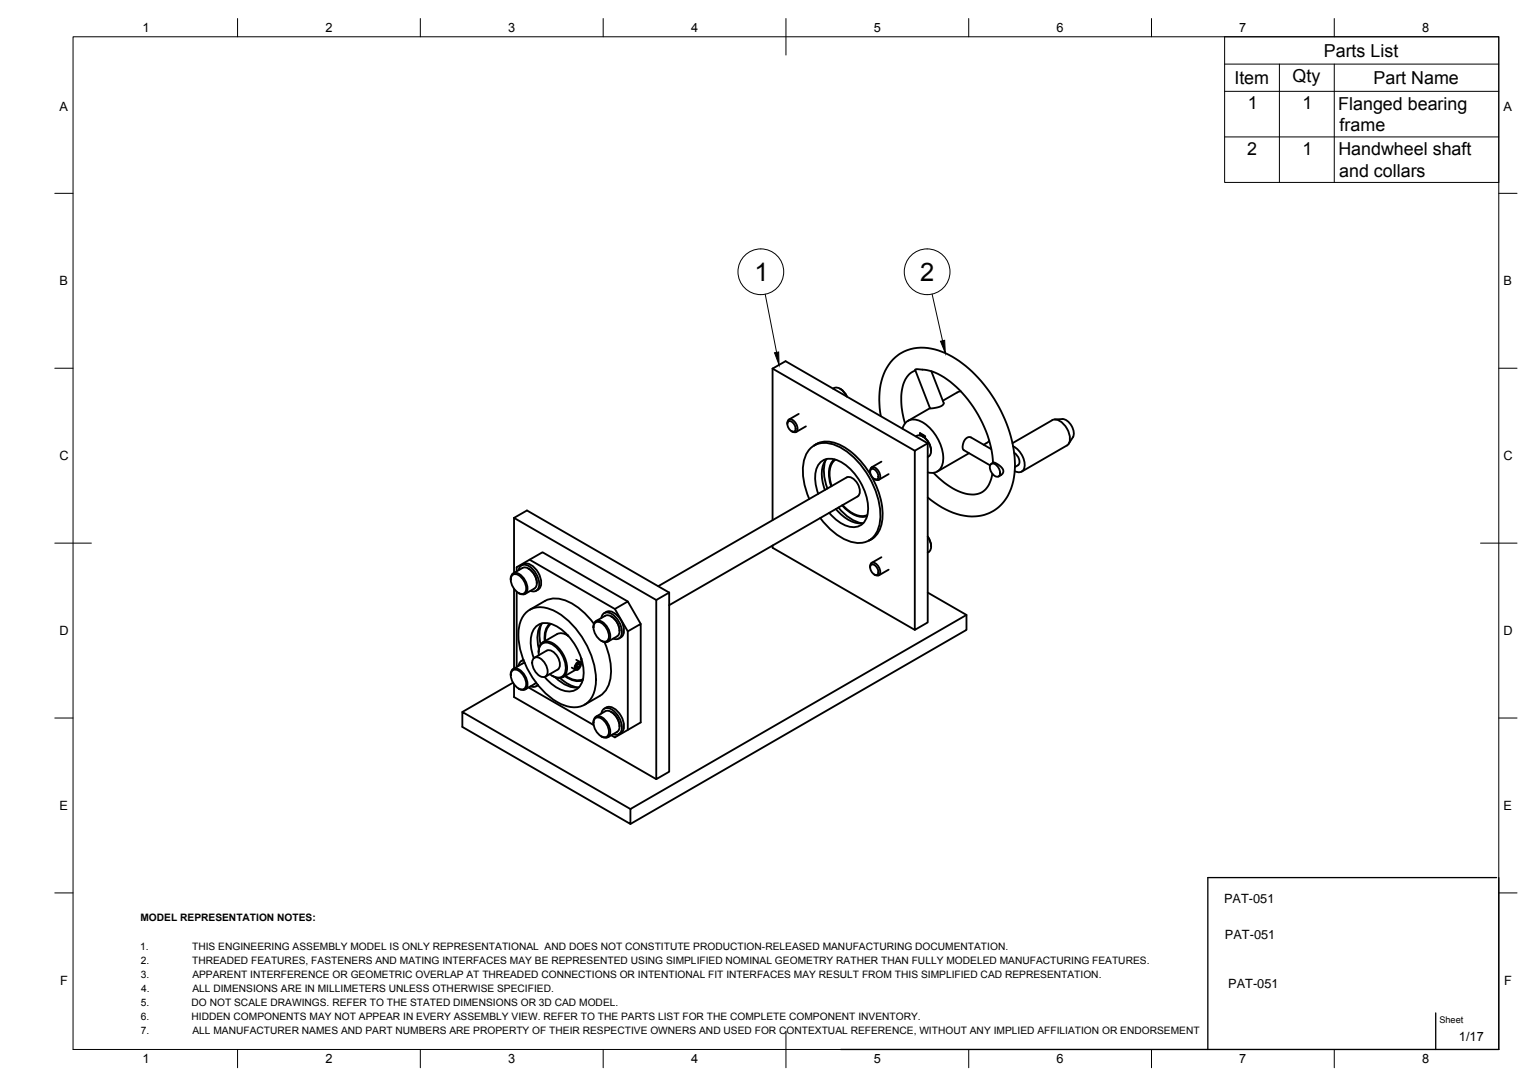
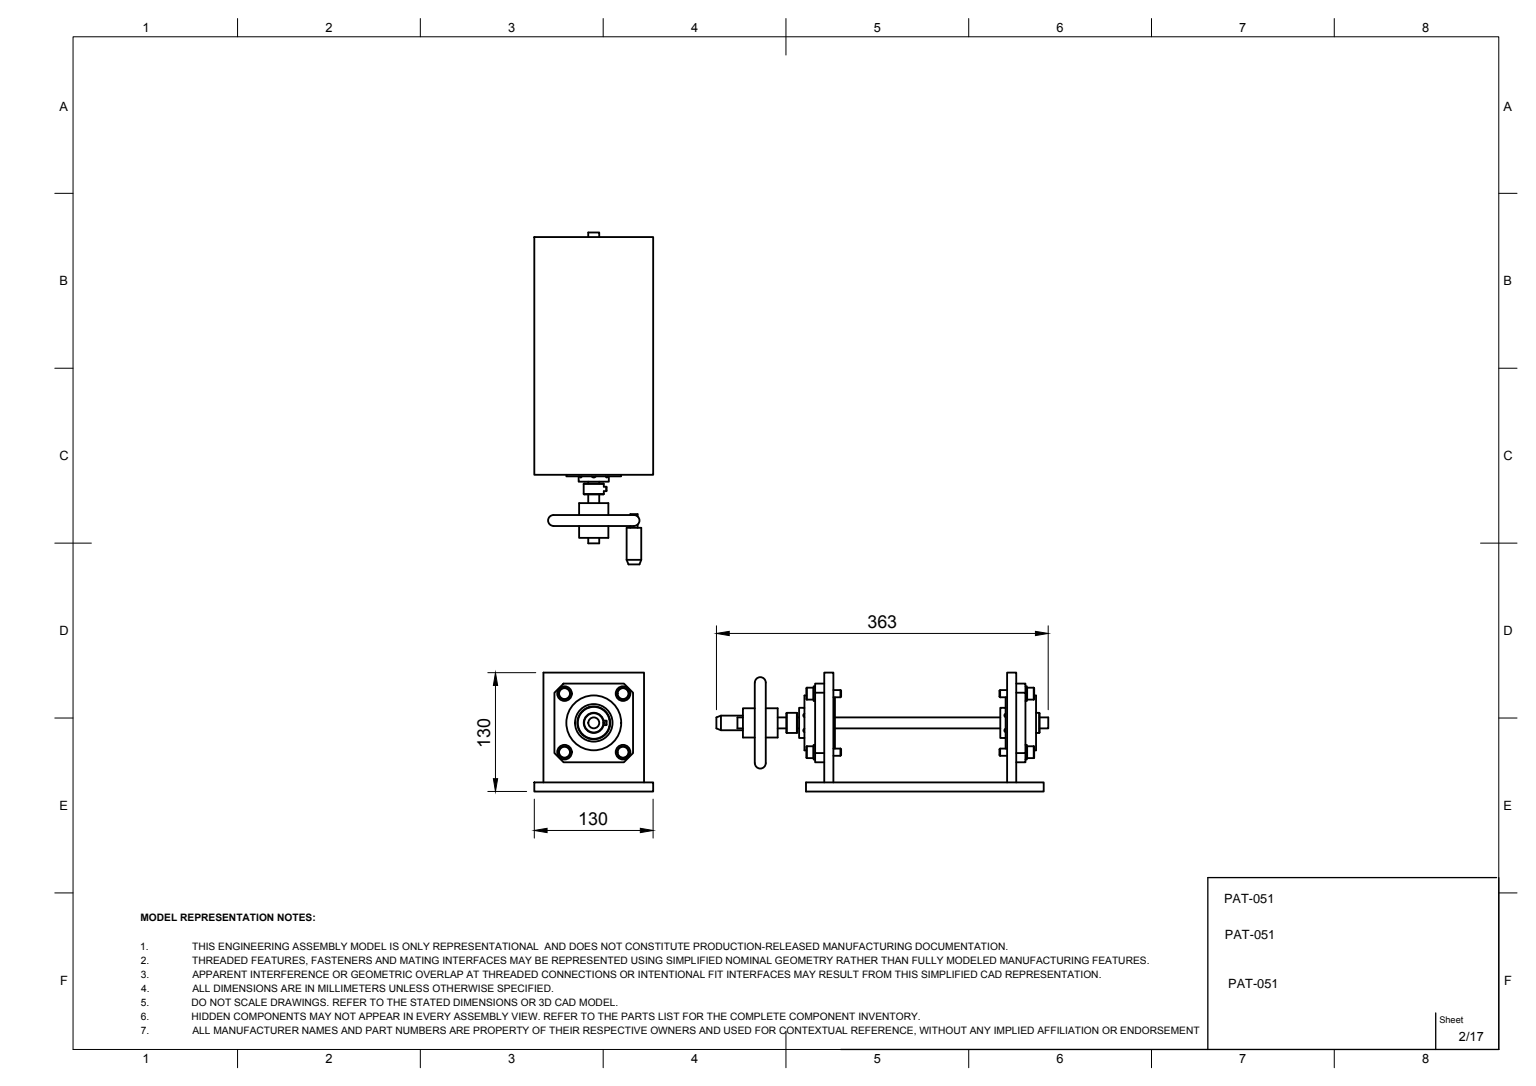
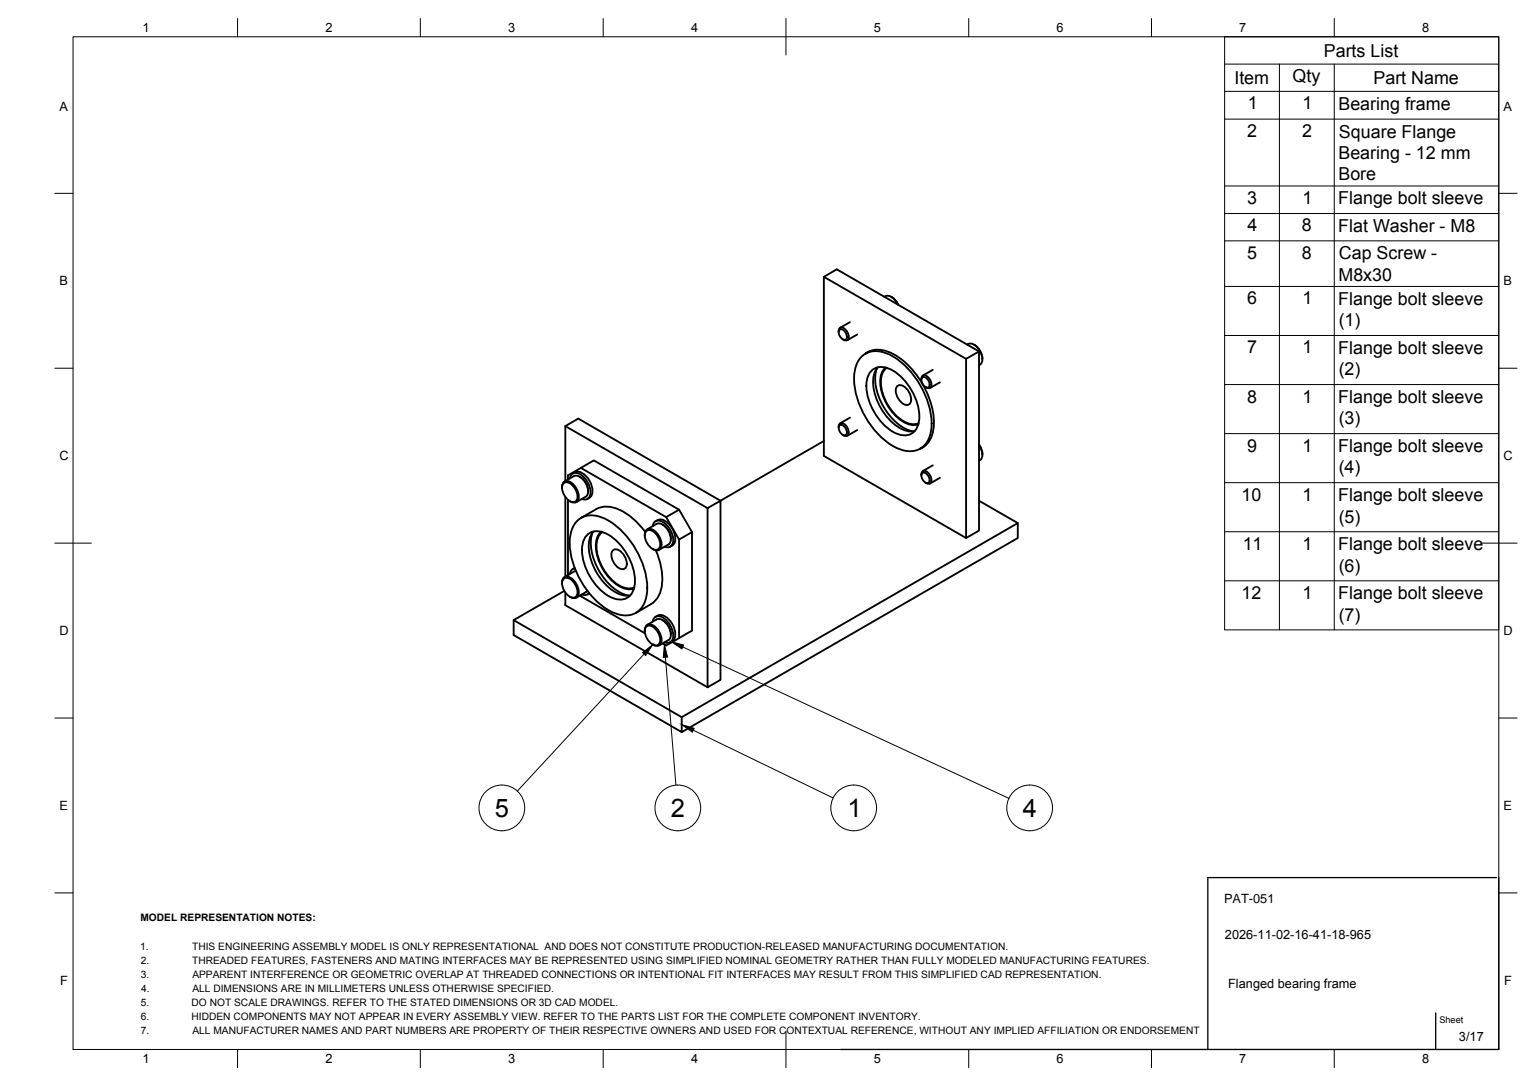
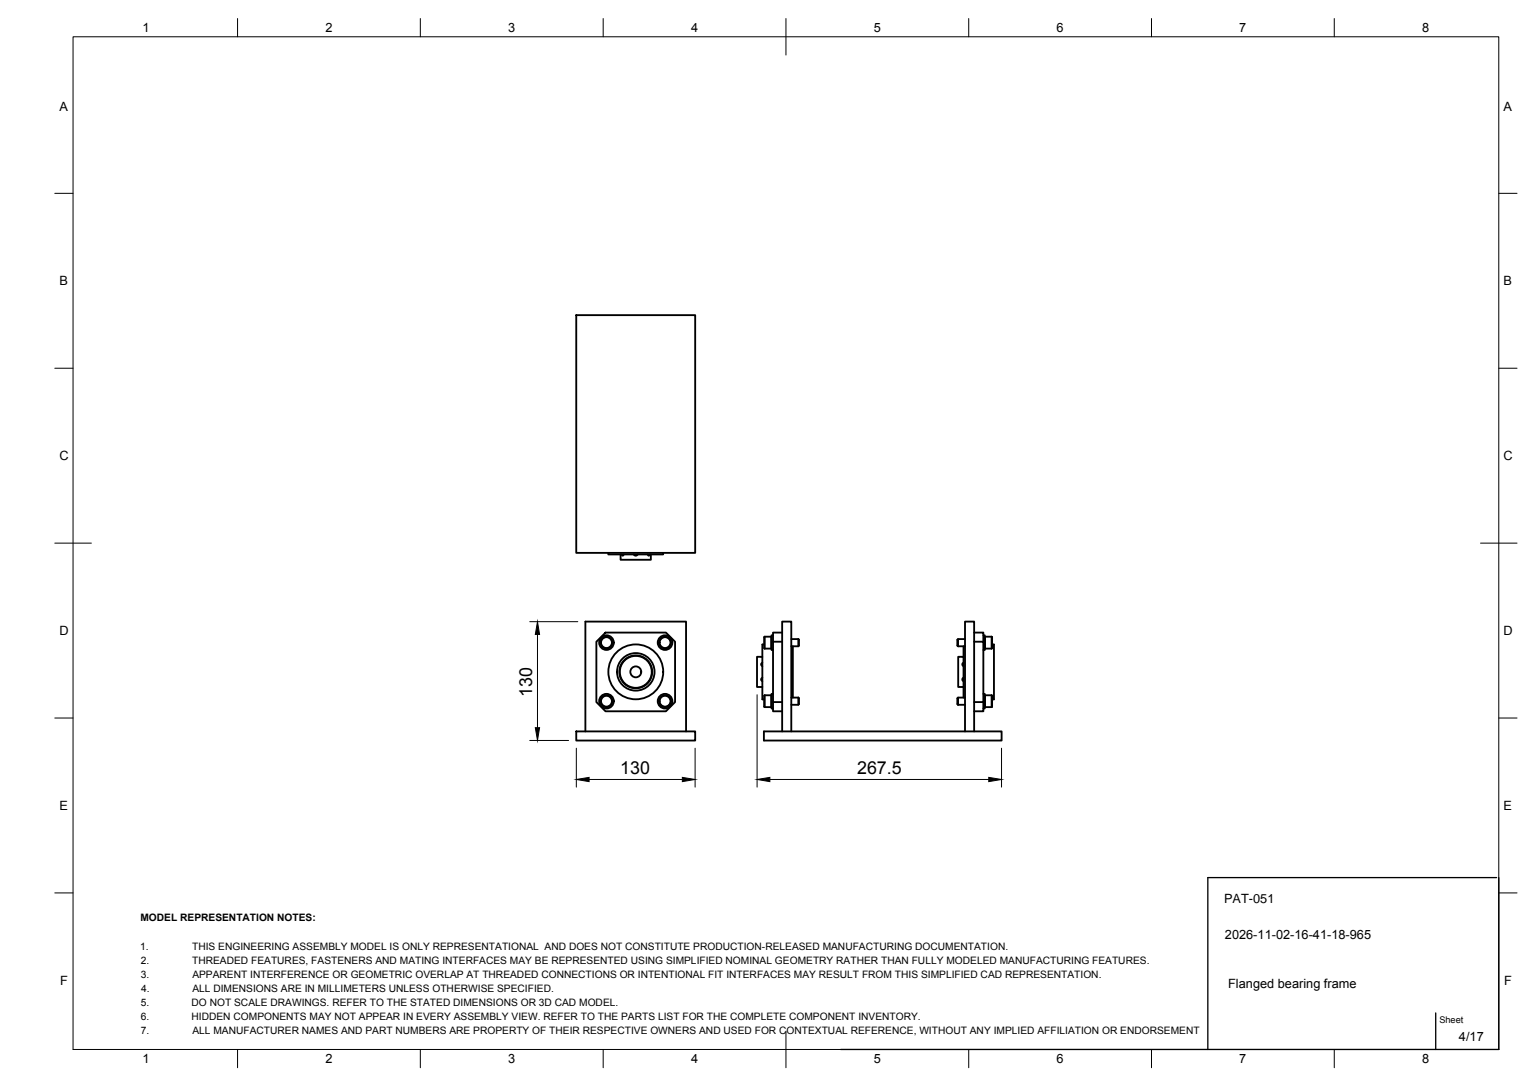
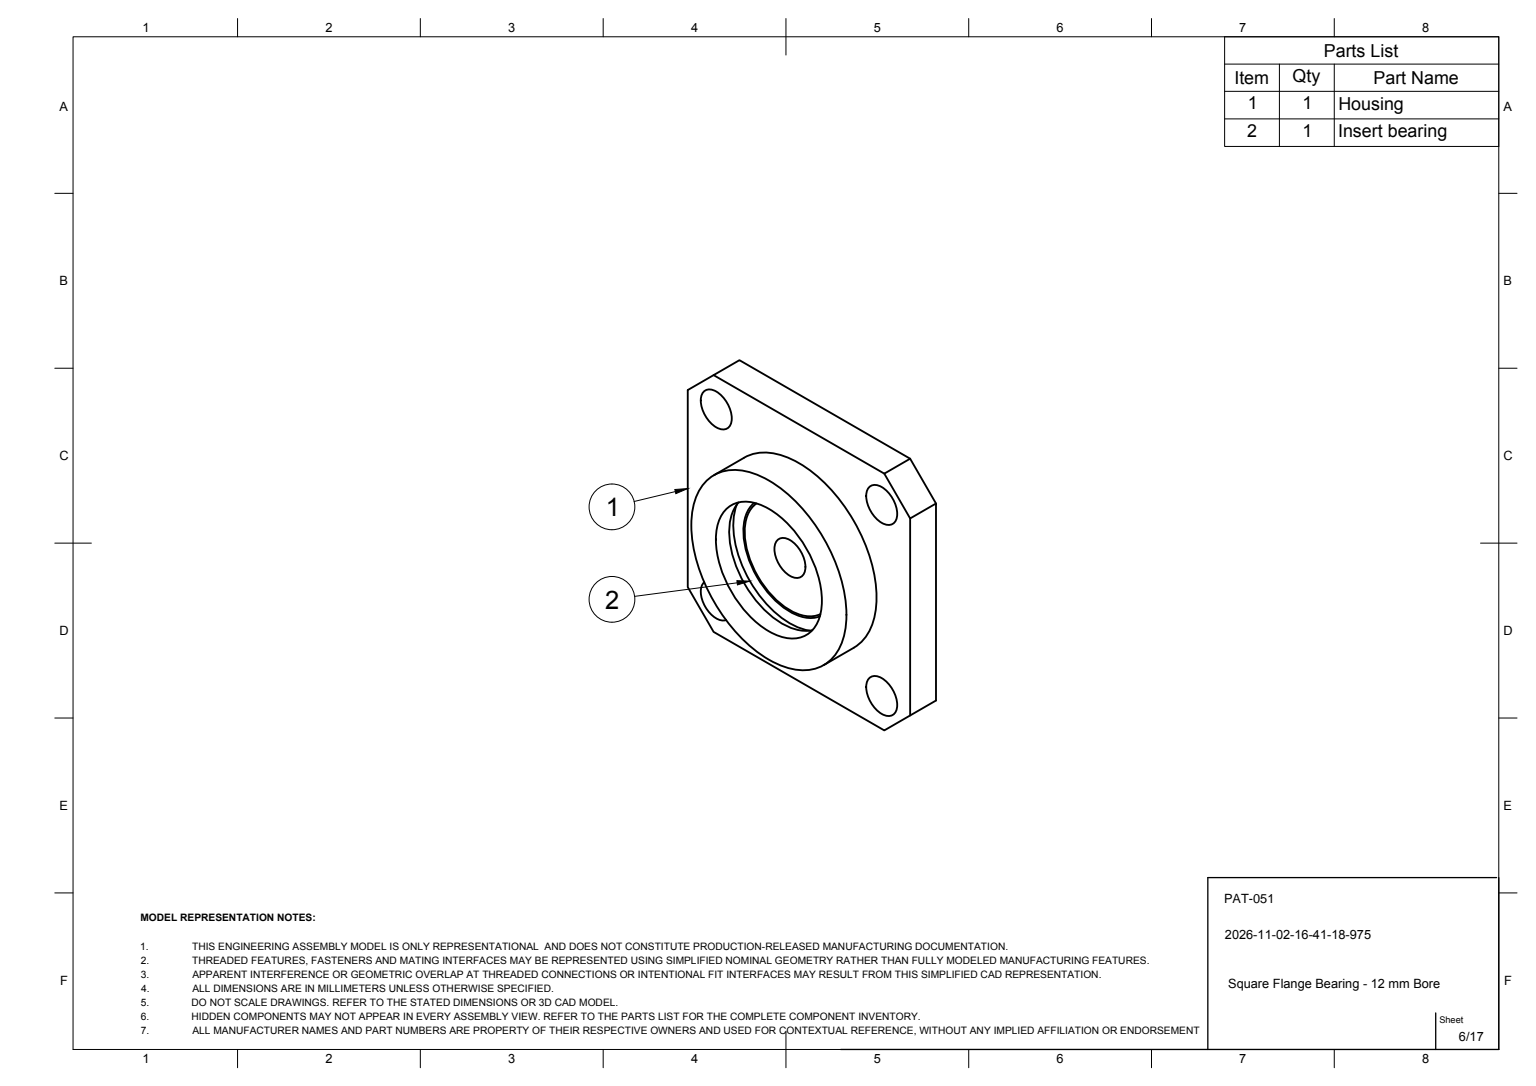
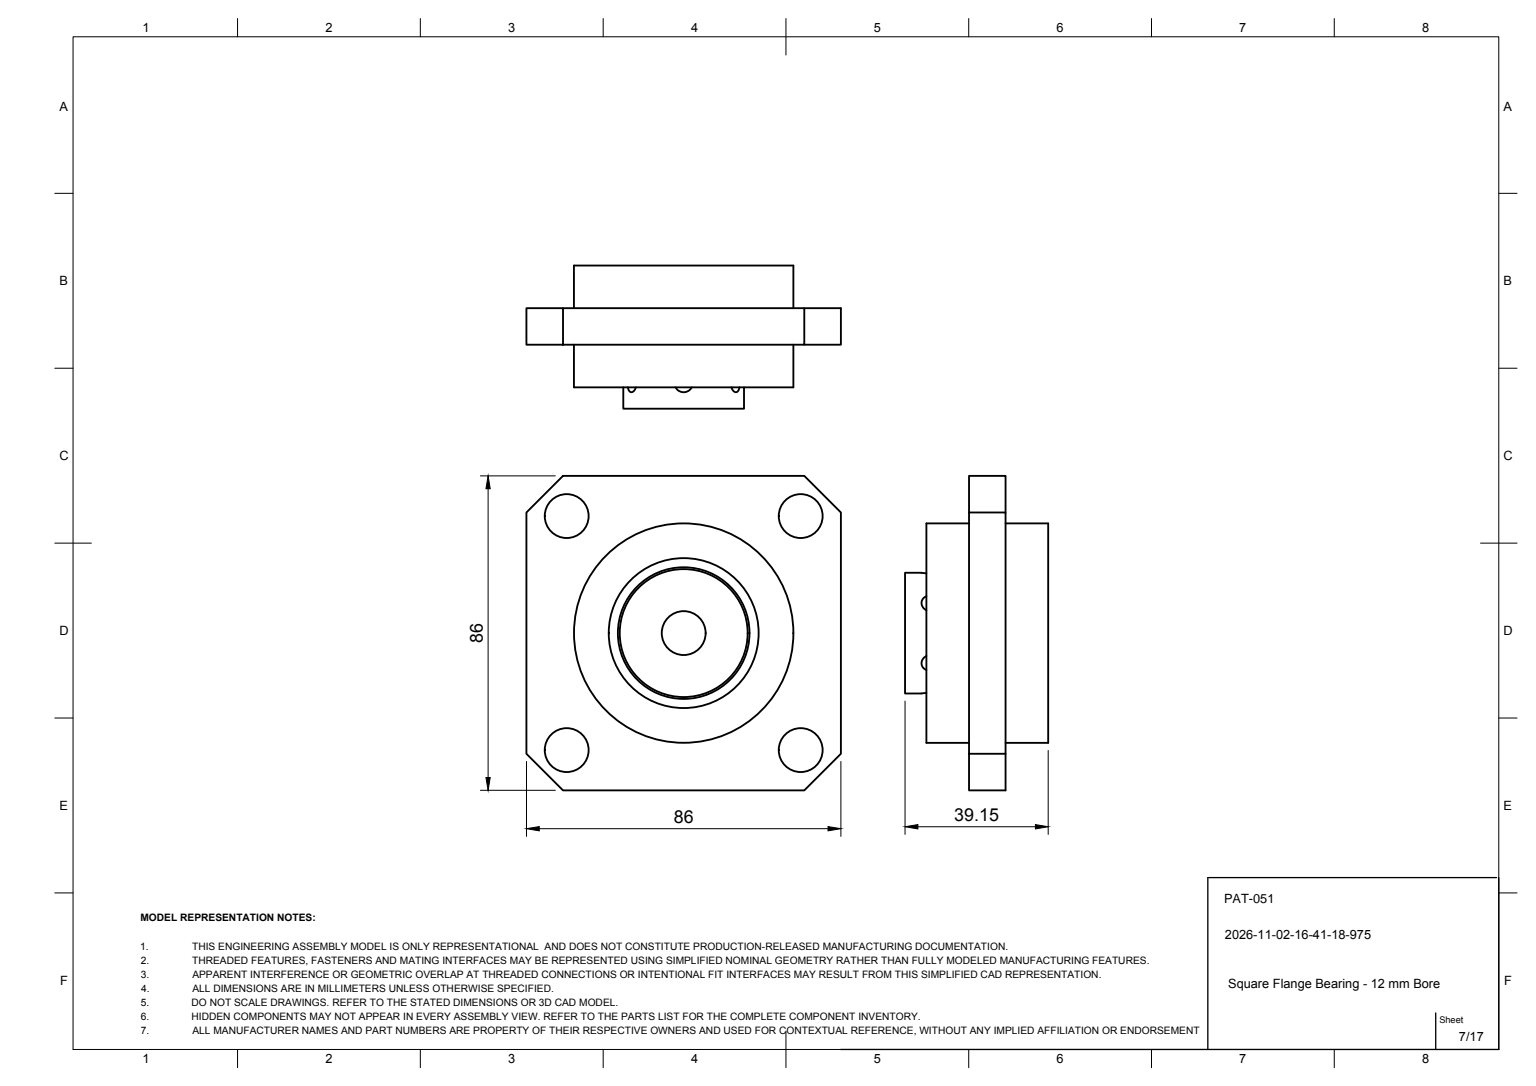
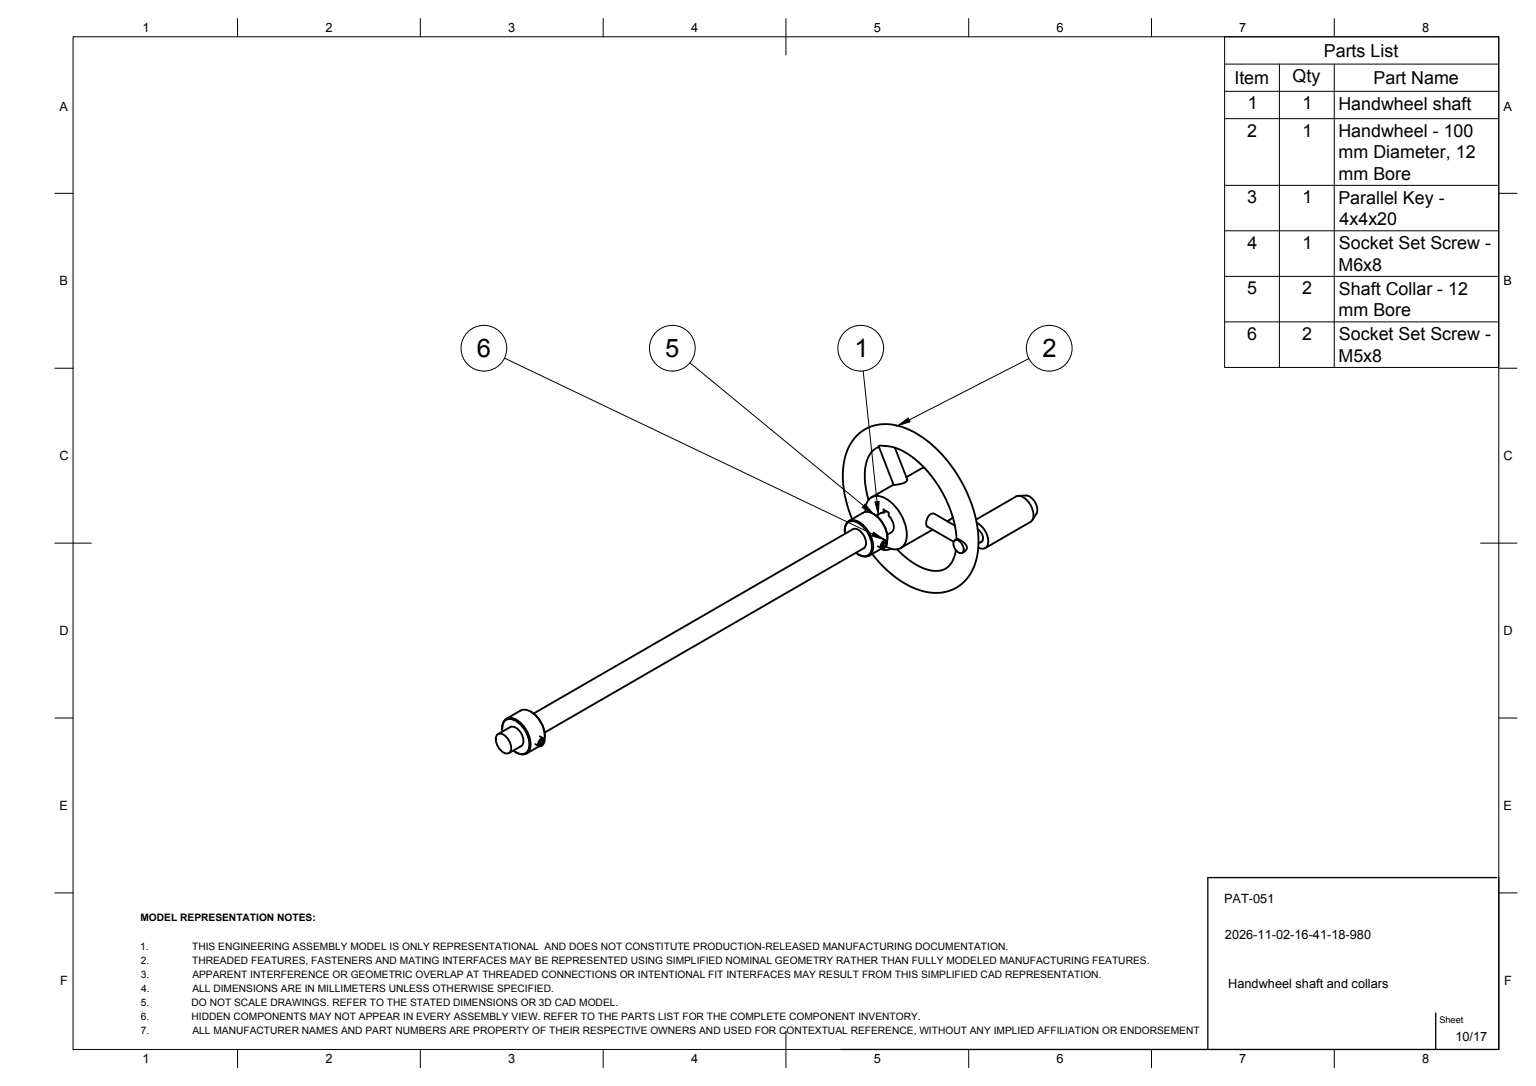
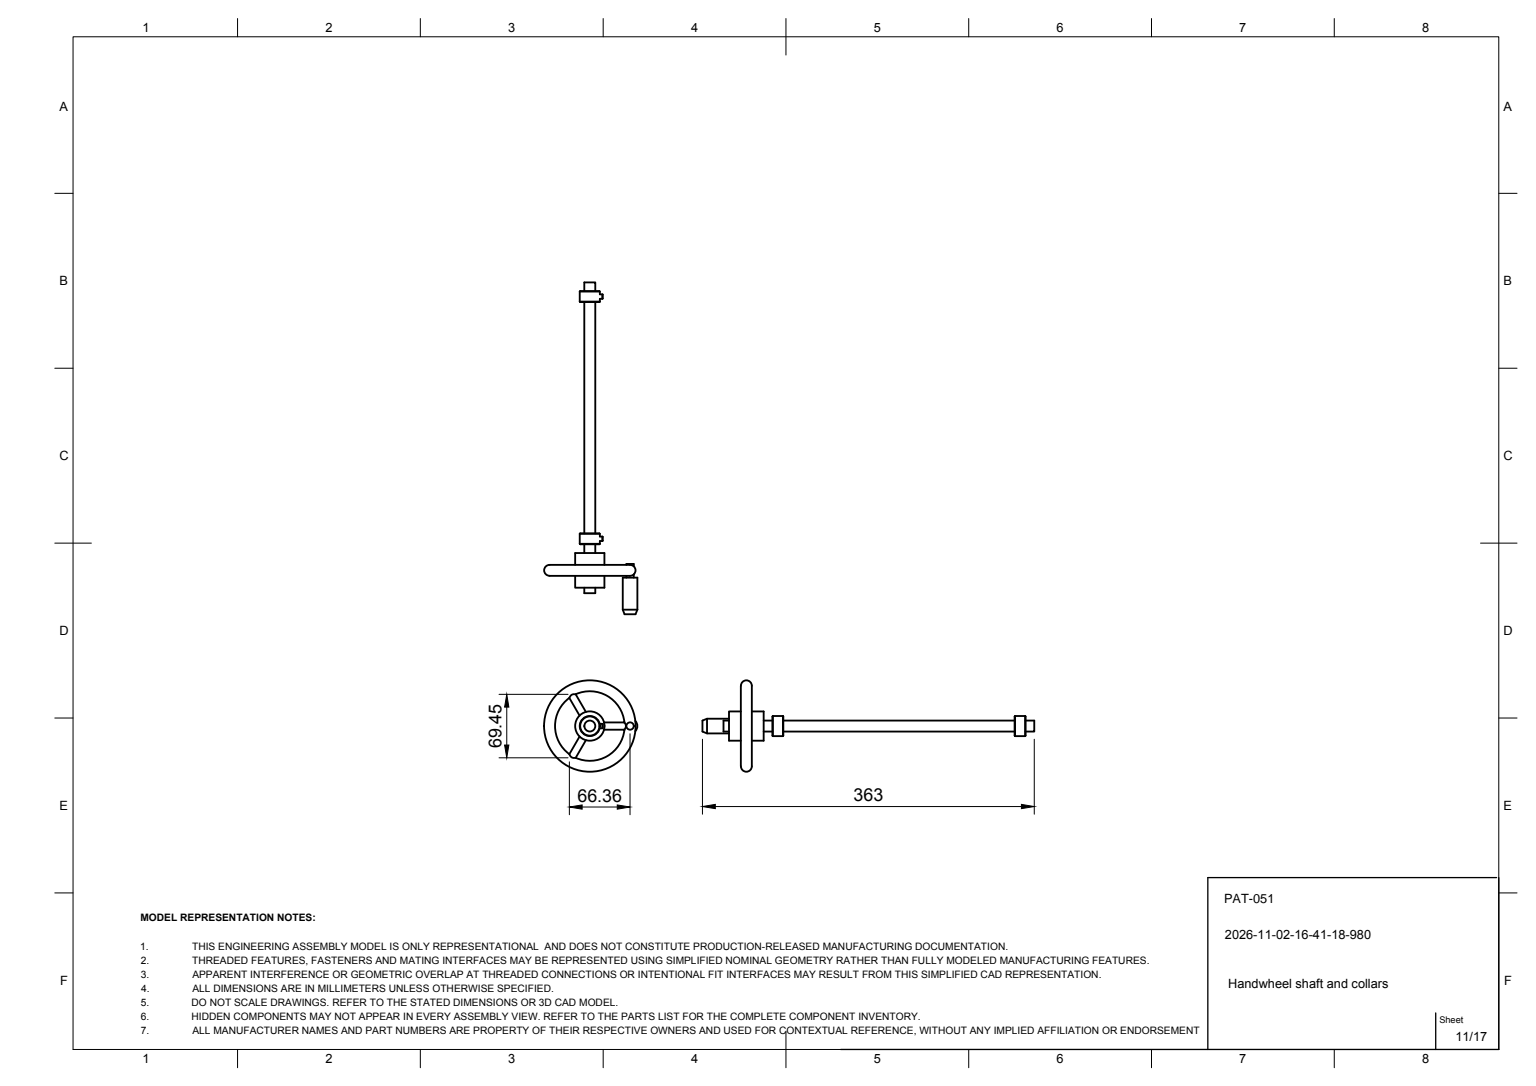
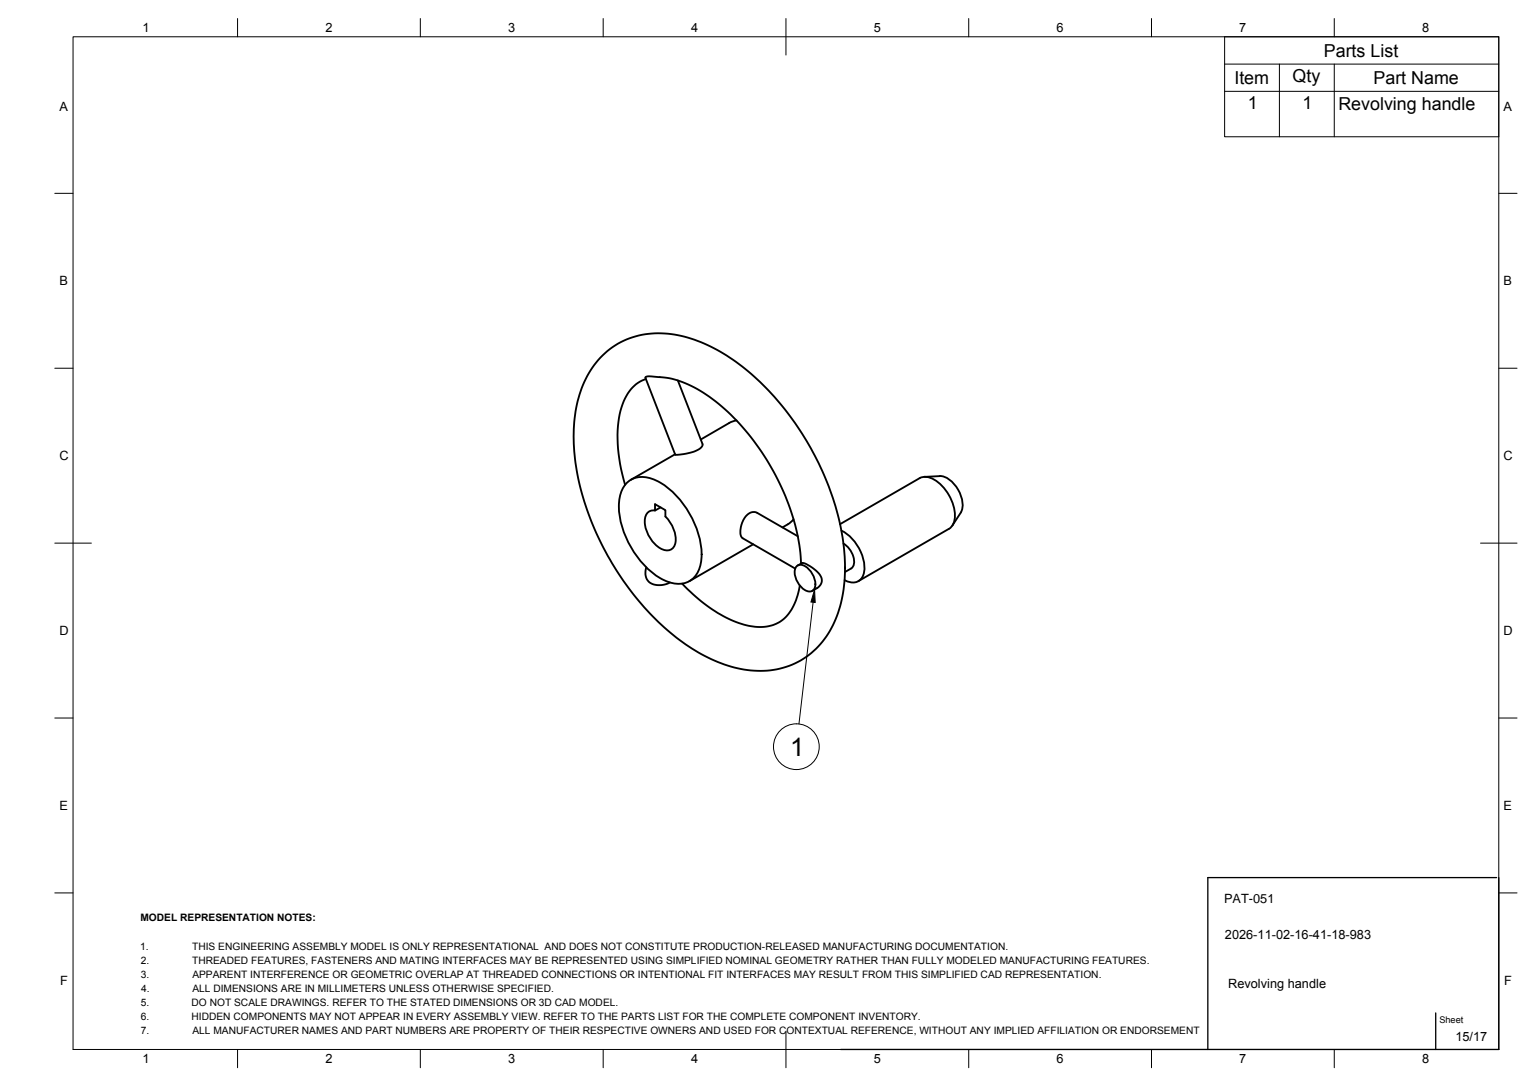
ISO-10303-21;
HEADER;
/* Generated by software containing ST-Developer
 * from STEP Tools, Inc. (www.steptools.com) 
 */

FILE_DESCRIPTION(
/* description */ ('Hand-crank flanged shaft unit'),
/* implementation_level */ '2;1');

FILE_NAME(
/* name */ 'PAT-051',
/* time_stamp */ '2026-10-27T18:35:45-07:00',
/* author */ (''),
/* organization */ (''),
/* preprocessor_version */ 'ST-DEVELOPER v20.2',
/* originating_system */ 'Autodesk Translation Framework v15.17.0.0',
/* authorisation */ '');

FILE_SCHEMA (('AUTOMOTIVE_DESIGN { 1 0 10303 214 3 1 1 }'));
ENDSEC;

DATA;
#10=MECHANICAL_DESIGN_GEOMETRIC_PRESENTATION_REPRESENTATION('',(#279,#280,
#281,#282,#283,#284,#285,#286,#287,#288,#289,#290,#291,#292,#293,#294,#295,
#296,#297,#298,#299),#6805);
#11=TOROIDAL_SURFACE('',#3848,4.4,0.6);
#12=ORIENTED_CLOSED_SHELL('',*,#3334,.F.);
#13=CONICAL_SURFACE('',#3755,0.625,0.785398163397448);
#14=CONICAL_SURFACE('',#3759,0.635,0.785398163397449);
#15=CONICAL_SURFACE('',#3763,0.41,0.463647609000806);
#16=CONICAL_SURFACE('',#3767,0.36,0.785398163397448);
#17=CONICAL_SURFACE('',#3823,0.699999999999999,0.380506377112365);
#18=CONICAL_SURFACE('',#3857,0.18,0.785398163397448);
#19=CONICAL_SURFACE('',#3861,0.18,0.785398163397448);
#20=CONICAL_SURFACE('',#3869,0.18,0.785398163397449);
#21=CONICAL_SURFACE('',#3872,0.18,0.785398163397449);
#22=CONICAL_SURFACE('',#3888,0.285,0.785398163397448);
#23=CONICAL_SURFACE('',#3892,0.25,0.785398163397448);
#24=CONICAL_SURFACE('',#3900,1.075,0.785398163397448);
#25=CONICAL_SURFACE('',#3904,1.075,0.785398163397449);
#26=CONICAL_SURFACE('',#3919,0.235,0.785398163397448);
#27=CONICAL_SURFACE('',#3923,0.2125,0.785398163397448);
#28=BREP_WITH_VOIDS('Body1',#3333,(#12));
#29=ITEM_DEFINED_TRANSFORMATION($,$,#3674,#3741);
#30=ITEM_DEFINED_TRANSFORMATION($,$,#3713,#3742);
#31=ITEM_DEFINED_TRANSFORMATION($,$,#3554,#3778);
#32=ITEM_DEFINED_TRANSFORMATION($,$,#3601,#3779);
#33=ITEM_DEFINED_TRANSFORMATION($,$,#3610,#3780);
#34=ITEM_DEFINED_TRANSFORMATION($,$,#3619,#3781);
#35=ITEM_DEFINED_TRANSFORMATION($,$,#3628,#3782);
#36=ITEM_DEFINED_TRANSFORMATION($,$,#3637,#3783);
#37=ITEM_DEFINED_TRANSFORMATION($,$,#3646,#3784);
#38=ITEM_DEFINED_TRANSFORMATION($,$,#3655,#3785);
#39=ITEM_DEFINED_TRANSFORMATION($,$,#3664,#3786);
#40=ITEM_DEFINED_TRANSFORMATION($,$,#3673,#3787);
#41=ITEM_DEFINED_TRANSFORMATION($,$,#3743,#3788);
#42=ITEM_DEFINED_TRANSFORMATION($,$,#3752,#3789);
#43=ITEM_DEFINED_TRANSFORMATION($,$,#3743,#3790);
#44=ITEM_DEFINED_TRANSFORMATION($,$,#3752,#3791);
#45=ITEM_DEFINED_TRANSFORMATION($,$,#3743,#3792);
#46=ITEM_DEFINED_TRANSFORMATION($,$,#3752,#3793);
#47=ITEM_DEFINED_TRANSFORMATION($,$,#3743,#3794);
#48=ITEM_DEFINED_TRANSFORMATION($,$,#3752,#3795);
#49=ITEM_DEFINED_TRANSFORMATION($,$,#3673,#3796);
#50=ITEM_DEFINED_TRANSFORMATION($,$,#3743,#3797);
#51=ITEM_DEFINED_TRANSFORMATION($,$,#3752,#3798);
#52=ITEM_DEFINED_TRANSFORMATION($,$,#3743,#3799);
#53=ITEM_DEFINED_TRANSFORMATION($,$,#3752,#3800);
#54=ITEM_DEFINED_TRANSFORMATION($,$,#3743,#3801);
#55=ITEM_DEFINED_TRANSFORMATION($,$,#3752,#3802);
#56=ITEM_DEFINED_TRANSFORMATION($,$,#3743,#3803);
#57=ITEM_DEFINED_TRANSFORMATION($,$,#3752,#3804);
#58=ITEM_DEFINED_TRANSFORMATION($,$,#3820,#3854);
#59=ITEM_DEFINED_TRANSFORMATION($,$,#3806,#3926);
#60=ITEM_DEFINED_TRANSFORMATION($,$,#3819,#3927);
#61=ITEM_DEFINED_TRANSFORMATION($,$,#3855,#3928);
#62=ITEM_DEFINED_TRANSFORMATION($,$,#3878,#3929);
#63=ITEM_DEFINED_TRANSFORMATION($,$,#3895,#3930);
#64=ITEM_DEFINED_TRANSFORMATION($,$,#3909,#3931);
#65=ITEM_DEFINED_TRANSFORMATION($,$,#3895,#3932);
#66=ITEM_DEFINED_TRANSFORMATION($,$,#3909,#3933);
#67=ITEM_DEFINED_TRANSFORMATION($,$,#3553,#3934);
#68=ITEM_DEFINED_TRANSFORMATION($,$,#3805,#3935);
#69=(
REPRESENTATION_RELATIONSHIP($,$,#6910,#6909)
REPRESENTATION_RELATIONSHIP_WITH_TRANSFORMATION(#29)
SHAPE_REPRESENTATION_RELATIONSHIP()
);
#70=(
REPRESENTATION_RELATIONSHIP($,$,#6911,#6909)
REPRESENTATION_RELATIONSHIP_WITH_TRANSFORMATION(#30)
SHAPE_REPRESENTATION_RELATIONSHIP()
);
#71=(
REPRESENTATION_RELATIONSHIP($,$,#6900,#6899)
REPRESENTATION_RELATIONSHIP_WITH_TRANSFORMATION(#31)
SHAPE_REPRESENTATION_RELATIONSHIP()
);
#72=(
REPRESENTATION_RELATIONSHIP($,$,#6901,#6899)
REPRESENTATION_RELATIONSHIP_WITH_TRANSFORMATION(#32)
SHAPE_REPRESENTATION_RELATIONSHIP()
);
#73=(
REPRESENTATION_RELATIONSHIP($,$,#6902,#6899)
REPRESENTATION_RELATIONSHIP_WITH_TRANSFORMATION(#33)
SHAPE_REPRESENTATION_RELATIONSHIP()
);
#74=(
REPRESENTATION_RELATIONSHIP($,$,#6903,#6899)
REPRESENTATION_RELATIONSHIP_WITH_TRANSFORMATION(#34)
SHAPE_REPRESENTATION_RELATIONSHIP()
);
#75=(
REPRESENTATION_RELATIONSHIP($,$,#6904,#6899)
REPRESENTATION_RELATIONSHIP_WITH_TRANSFORMATION(#35)
SHAPE_REPRESENTATION_RELATIONSHIP()
);
#76=(
REPRESENTATION_RELATIONSHIP($,$,#6905,#6899)
REPRESENTATION_RELATIONSHIP_WITH_TRANSFORMATION(#36)
SHAPE_REPRESENTATION_RELATIONSHIP()
);
#77=(
REPRESENTATION_RELATIONSHIP($,$,#6906,#6899)
REPRESENTATION_RELATIONSHIP_WITH_TRANSFORMATION(#37)
SHAPE_REPRESENTATION_RELATIONSHIP()
);
#78=(
REPRESENTATION_RELATIONSHIP($,$,#6907,#6899)
REPRESENTATION_RELATIONSHIP_WITH_TRANSFORMATION(#38)
SHAPE_REPRESENTATION_RELATIONSHIP()
);
#79=(
REPRESENTATION_RELATIONSHIP($,$,#6908,#6899)
REPRESENTATION_RELATIONSHIP_WITH_TRANSFORMATION(#39)
SHAPE_REPRESENTATION_RELATIONSHIP()
);
#80=(
REPRESENTATION_RELATIONSHIP($,$,#6909,#6899)
REPRESENTATION_RELATIONSHIP_WITH_TRANSFORMATION(#40)
SHAPE_REPRESENTATION_RELATIONSHIP()
);
#81=(
REPRESENTATION_RELATIONSHIP($,$,#6912,#6899)
REPRESENTATION_RELATIONSHIP_WITH_TRANSFORMATION(#41)
SHAPE_REPRESENTATION_RELATIONSHIP()
);
#82=(
REPRESENTATION_RELATIONSHIP($,$,#6913,#6899)
REPRESENTATION_RELATIONSHIP_WITH_TRANSFORMATION(#42)
SHAPE_REPRESENTATION_RELATIONSHIP()
);
#83=(
REPRESENTATION_RELATIONSHIP($,$,#6912,#6899)
REPRESENTATION_RELATIONSHIP_WITH_TRANSFORMATION(#43)
SHAPE_REPRESENTATION_RELATIONSHIP()
);
#84=(
REPRESENTATION_RELATIONSHIP($,$,#6913,#6899)
REPRESENTATION_RELATIONSHIP_WITH_TRANSFORMATION(#44)
SHAPE_REPRESENTATION_RELATIONSHIP()
);
#85=(
REPRESENTATION_RELATIONSHIP($,$,#6912,#6899)
REPRESENTATION_RELATIONSHIP_WITH_TRANSFORMATION(#45)
SHAPE_REPRESENTATION_RELATIONSHIP()
);
#86=(
REPRESENTATION_RELATIONSHIP($,$,#6913,#6899)
REPRESENTATION_RELATIONSHIP_WITH_TRANSFORMATION(#46)
SHAPE_REPRESENTATION_RELATIONSHIP()
);
#87=(
REPRESENTATION_RELATIONSHIP($,$,#6912,#6899)
REPRESENTATION_RELATIONSHIP_WITH_TRANSFORMATION(#47)
SHAPE_REPRESENTATION_RELATIONSHIP()
);
#88=(
REPRESENTATION_RELATIONSHIP($,$,#6913,#6899)
REPRESENTATION_RELATIONSHIP_WITH_TRANSFORMATION(#48)
SHAPE_REPRESENTATION_RELATIONSHIP()
);
#89=(
REPRESENTATION_RELATIONSHIP($,$,#6909,#6899)
REPRESENTATION_RELATIONSHIP_WITH_TRANSFORMATION(#49)
SHAPE_REPRESENTATION_RELATIONSHIP()
);
#90=(
REPRESENTATION_RELATIONSHIP($,$,#6912,#6899)
REPRESENTATION_RELATIONSHIP_WITH_TRANSFORMATION(#50)
SHAPE_REPRESENTATION_RELATIONSHIP()
);
#91=(
REPRESENTATION_RELATIONSHIP($,$,#6913,#6899)
REPRESENTATION_RELATIONSHIP_WITH_TRANSFORMATION(#51)
SHAPE_REPRESENTATION_RELATIONSHIP()
);
#92=(
REPRESENTATION_RELATIONSHIP($,$,#6912,#6899)
REPRESENTATION_RELATIONSHIP_WITH_TRANSFORMATION(#52)
SHAPE_REPRESENTATION_RELATIONSHIP()
);
#93=(
REPRESENTATION_RELATIONSHIP($,$,#6913,#6899)
REPRESENTATION_RELATIONSHIP_WITH_TRANSFORMATION(#53)
SHAPE_REPRESENTATION_RELATIONSHIP()
);
#94=(
REPRESENTATION_RELATIONSHIP($,$,#6912,#6899)
REPRESENTATION_RELATIONSHIP_WITH_TRANSFORMATION(#54)
SHAPE_REPRESENTATION_RELATIONSHIP()
);
#95=(
REPRESENTATION_RELATIONSHIP($,$,#6913,#6899)
REPRESENTATION_RELATIONSHIP_WITH_TRANSFORMATION(#55)
SHAPE_REPRESENTATION_RELATIONSHIP()
);
#96=(
REPRESENTATION_RELATIONSHIP($,$,#6912,#6899)
REPRESENTATION_RELATIONSHIP_WITH_TRANSFORMATION(#56)
SHAPE_REPRESENTATION_RELATIONSHIP()
);
#97=(
REPRESENTATION_RELATIONSHIP($,$,#6913,#6899)
REPRESENTATION_RELATIONSHIP_WITH_TRANSFORMATION(#57)
SHAPE_REPRESENTATION_RELATIONSHIP()
);
#98=(
REPRESENTATION_RELATIONSHIP($,$,#6917,#6916)
REPRESENTATION_RELATIONSHIP_WITH_TRANSFORMATION(#58)
SHAPE_REPRESENTATION_RELATIONSHIP()
);
#99=(
REPRESENTATION_RELATIONSHIP($,$,#6915,#6914)
REPRESENTATION_RELATIONSHIP_WITH_TRANSFORMATION(#59)
SHAPE_REPRESENTATION_RELATIONSHIP()
);
#100=(
REPRESENTATION_RELATIONSHIP($,$,#6916,#6914)
REPRESENTATION_RELATIONSHIP_WITH_TRANSFORMATION(#60)
SHAPE_REPRESENTATION_RELATIONSHIP()
);
#101=(
REPRESENTATION_RELATIONSHIP($,$,#6918,#6914)
REPRESENTATION_RELATIONSHIP_WITH_TRANSFORMATION(#61)
SHAPE_REPRESENTATION_RELATIONSHIP()
);
#102=(
REPRESENTATION_RELATIONSHIP($,$,#6919,#6914)
REPRESENTATION_RELATIONSHIP_WITH_TRANSFORMATION(#62)
SHAPE_REPRESENTATION_RELATIONSHIP()
);
#103=(
REPRESENTATION_RELATIONSHIP($,$,#6920,#6914)
REPRESENTATION_RELATIONSHIP_WITH_TRANSFORMATION(#63)
SHAPE_REPRESENTATION_RELATIONSHIP()
);
#104=(
REPRESENTATION_RELATIONSHIP($,$,#6921,#6914)
REPRESENTATION_RELATIONSHIP_WITH_TRANSFORMATION(#64)
SHAPE_REPRESENTATION_RELATIONSHIP()
);
#105=(
REPRESENTATION_RELATIONSHIP($,$,#6920,#6914)
REPRESENTATION_RELATIONSHIP_WITH_TRANSFORMATION(#65)
SHAPE_REPRESENTATION_RELATIONSHIP()
);
#106=(
REPRESENTATION_RELATIONSHIP($,$,#6921,#6914)
REPRESENTATION_RELATIONSHIP_WITH_TRANSFORMATION(#66)
SHAPE_REPRESENTATION_RELATIONSHIP()
);
#107=(
REPRESENTATION_RELATIONSHIP($,$,#6899,#6898)
REPRESENTATION_RELATIONSHIP_WITH_TRANSFORMATION(#67)
SHAPE_REPRESENTATION_RELATIONSHIP()
);
#108=(
REPRESENTATION_RELATIONSHIP($,$,#6914,#6898)
REPRESENTATION_RELATIONSHIP_WITH_TRANSFORMATION(#68)
SHAPE_REPRESENTATION_RELATIONSHIP()
);
#109=CONTEXT_DEPENDENT_SHAPE_REPRESENTATION(#69,#6848);
#110=CONTEXT_DEPENDENT_SHAPE_REPRESENTATION(#70,#6849);
#111=CONTEXT_DEPENDENT_SHAPE_REPRESENTATION(#71,#6852);
#112=CONTEXT_DEPENDENT_SHAPE_REPRESENTATION(#72,#6853);
#113=CONTEXT_DEPENDENT_SHAPE_REPRESENTATION(#73,#6854);
#114=CONTEXT_DEPENDENT_SHAPE_REPRESENTATION(#74,#6855);
#115=CONTEXT_DEPENDENT_SHAPE_REPRESENTATION(#75,#6856);
#116=CONTEXT_DEPENDENT_SHAPE_REPRESENTATION(#76,#6857);
#117=CONTEXT_DEPENDENT_SHAPE_REPRESENTATION(#77,#6858);
#118=CONTEXT_DEPENDENT_SHAPE_REPRESENTATION(#78,#6859);
#119=CONTEXT_DEPENDENT_SHAPE_REPRESENTATION(#79,#6860);
#120=CONTEXT_DEPENDENT_SHAPE_REPRESENTATION(#80,#6861);
#121=CONTEXT_DEPENDENT_SHAPE_REPRESENTATION(#81,#6862);
#122=CONTEXT_DEPENDENT_SHAPE_REPRESENTATION(#82,#6863);
#123=CONTEXT_DEPENDENT_SHAPE_REPRESENTATION(#83,#6864);
#124=CONTEXT_DEPENDENT_SHAPE_REPRESENTATION(#84,#6865);
#125=CONTEXT_DEPENDENT_SHAPE_REPRESENTATION(#85,#6866);
#126=CONTEXT_DEPENDENT_SHAPE_REPRESENTATION(#86,#6867);
#127=CONTEXT_DEPENDENT_SHAPE_REPRESENTATION(#87,#6868);
#128=CONTEXT_DEPENDENT_SHAPE_REPRESENTATION(#88,#6869);
#129=CONTEXT_DEPENDENT_SHAPE_REPRESENTATION(#89,#6870);
#130=CONTEXT_DEPENDENT_SHAPE_REPRESENTATION(#90,#6871);
#131=CONTEXT_DEPENDENT_SHAPE_REPRESENTATION(#91,#6872);
#132=CONTEXT_DEPENDENT_SHAPE_REPRESENTATION(#92,#6873);
#133=CONTEXT_DEPENDENT_SHAPE_REPRESENTATION(#93,#6874);
#134=CONTEXT_DEPENDENT_SHAPE_REPRESENTATION(#94,#6875);
#135=CONTEXT_DEPENDENT_SHAPE_REPRESENTATION(#95,#6876);
#136=CONTEXT_DEPENDENT_SHAPE_REPRESENTATION(#96,#6877);
#137=CONTEXT_DEPENDENT_SHAPE_REPRESENTATION(#97,#6878);
#138=CONTEXT_DEPENDENT_SHAPE_REPRESENTATION(#98,#6883);
#139=CONTEXT_DEPENDENT_SHAPE_REPRESENTATION(#99,#6888);
#140=CONTEXT_DEPENDENT_SHAPE_REPRESENTATION(#100,#6889);
#141=CONTEXT_DEPENDENT_SHAPE_REPRESENTATION(#101,#6890);
#142=CONTEXT_DEPENDENT_SHAPE_REPRESENTATION(#102,#6891);
#143=CONTEXT_DEPENDENT_SHAPE_REPRESENTATION(#103,#6892);
#144=CONTEXT_DEPENDENT_SHAPE_REPRESENTATION(#104,#6893);
#145=CONTEXT_DEPENDENT_SHAPE_REPRESENTATION(#105,#6894);
#146=CONTEXT_DEPENDENT_SHAPE_REPRESENTATION(#106,#6895);
#147=CONTEXT_DEPENDENT_SHAPE_REPRESENTATION(#107,#6896);
#148=CONTEXT_DEPENDENT_SHAPE_REPRESENTATION(#108,#6897);
#149=NEXT_ASSEMBLY_USAGE_OCCURRENCE('Housing:1','Housing:1','Housing:1',
#6934,#6935,'Housing:1');
#150=NEXT_ASSEMBLY_USAGE_OCCURRENCE('Insert bearing:1',
'Insert bearing:1','Insert bearing:1',#6934,#6936,'Insert bearing:1');
#151=NEXT_ASSEMBLY_USAGE_OCCURRENCE('Bearing frame:1','Bearing frame:1',
'Bearing frame:1',#6924,#6925,'Bearing frame:1');
#152=NEXT_ASSEMBLY_USAGE_OCCURRENCE('Flange bolt sleeve:1',
'Flange bolt sleeve:1','Flange bolt sleeve:1',#6924,#6926,
'Flange bolt sleeve:1');
#153=NEXT_ASSEMBLY_USAGE_OCCURRENCE('Flange bolt sleeve (1):1',
'Flange bolt sleeve (1):1','Flange bolt sleeve (1):1',#6924,#6927,
'Flange bolt sleeve (1):1');
#154=NEXT_ASSEMBLY_USAGE_OCCURRENCE('Flange bolt sleeve (2):1',
'Flange bolt sleeve (2):1','Flange bolt sleeve (2):1',#6924,#6928,
'Flange bolt sleeve (2):1');
#155=NEXT_ASSEMBLY_USAGE_OCCURRENCE('Flange bolt sleeve (3):1',
'Flange bolt sleeve (3):1','Flange bolt sleeve (3):1',#6924,#6929,
'Flange bolt sleeve (3):1');
#156=NEXT_ASSEMBLY_USAGE_OCCURRENCE('Flange bolt sleeve (4):1',
'Flange bolt sleeve (4):1','Flange bolt sleeve (4):1',#6924,#6930,
'Flange bolt sleeve (4):1');
#157=NEXT_ASSEMBLY_USAGE_OCCURRENCE('Flange bolt sleeve (5):1',
'Flange bolt sleeve (5):1','Flange bolt sleeve (5):1',#6924,#6931,
'Flange bolt sleeve (5):1');
#158=NEXT_ASSEMBLY_USAGE_OCCURRENCE('Flange bolt sleeve (6):1',
'Flange bolt sleeve (6):1','Flange bolt sleeve (6):1',#6924,#6932,
'Flange bolt sleeve (6):1');
#159=NEXT_ASSEMBLY_USAGE_OCCURRENCE('Flange bolt sleeve (7):1',
'Flange bolt sleeve (7):1','Flange bolt sleeve (7):1',#6924,#6933,
'Flange bolt sleeve (7):1');
#160=NEXT_ASSEMBLY_USAGE_OCCURRENCE(
'Square Flange Bearing - 12 mm Bore:2',
'Square Flange Bearing - 12 mm Bore:2',
'Square Flange Bearing - 12 mm Bore:2',#6924,#6934,
'Square Flange Bearing - 12 mm Bore:2');
#161=NEXT_ASSEMBLY_USAGE_OCCURRENCE('Flat Washer - M8:2',
'Flat Washer - M8:2','Flat Washer - M8:2',#6924,#6937,
'Flat Washer - M8:2');
#162=NEXT_ASSEMBLY_USAGE_OCCURRENCE('Cap Screw - M8x30:2',
'Cap Screw - M8x30:2','Cap Screw - M8x30:2',#6924,#6938,
'Cap Screw - M8x30:2');
#163=NEXT_ASSEMBLY_USAGE_OCCURRENCE('Flat Washer - M8:3',
'Flat Washer - M8:3','Flat Washer - M8:3',#6924,#6937,
'Flat Washer - M8:3');
#164=NEXT_ASSEMBLY_USAGE_OCCURRENCE('Cap Screw - M8x30:3',
'Cap Screw - M8x30:3','Cap Screw - M8x30:3',#6924,#6938,
'Cap Screw - M8x30:3');
#165=NEXT_ASSEMBLY_USAGE_OCCURRENCE('Flat Washer - M8:4',
'Flat Washer - M8:4','Flat Washer - M8:4',#6924,#6937,
'Flat Washer - M8:4');
#166=NEXT_ASSEMBLY_USAGE_OCCURRENCE('Cap Screw - M8x30:4',
'Cap Screw - M8x30:4','Cap Screw - M8x30:4',#6924,#6938,
'Cap Screw - M8x30:4');
#167=NEXT_ASSEMBLY_USAGE_OCCURRENCE('Flat Washer - M8:5',
'Flat Washer - M8:5','Flat Washer - M8:5',#6924,#6937,
'Flat Washer - M8:5');
#168=NEXT_ASSEMBLY_USAGE_OCCURRENCE('Cap Screw - M8x30:5',
'Cap Screw - M8x30:5','Cap Screw - M8x30:5',#6924,#6938,
'Cap Screw - M8x30:5');
#169=NEXT_ASSEMBLY_USAGE_OCCURRENCE(
'Square Flange Bearing - 12 mm Bore:3',
'Square Flange Bearing - 12 mm Bore:3',
'Square Flange Bearing - 12 mm Bore:3',#6924,#6934,
'Square Flange Bearing - 12 mm Bore:3');
#170=NEXT_ASSEMBLY_USAGE_OCCURRENCE('Flat Washer - M8:6',
'Flat Washer - M8:6','Flat Washer - M8:6',#6924,#6937,
'Flat Washer - M8:6');
#171=NEXT_ASSEMBLY_USAGE_OCCURRENCE('Cap Screw - M8x30:6',
'Cap Screw - M8x30:6','Cap Screw - M8x30:6',#6924,#6938,
'Cap Screw - M8x30:6');
#172=NEXT_ASSEMBLY_USAGE_OCCURRENCE('Flat Washer - M8:7',
'Flat Washer - M8:7','Flat Washer - M8:7',#6924,#6937,
'Flat Washer - M8:7');
#173=NEXT_ASSEMBLY_USAGE_OCCURRENCE('Cap Screw - M8x30:7',
'Cap Screw - M8x30:7','Cap Screw - M8x30:7',#6924,#6938,
'Cap Screw - M8x30:7');
#174=NEXT_ASSEMBLY_USAGE_OCCURRENCE('Flat Washer - M8:8',
'Flat Washer - M8:8','Flat Washer - M8:8',#6924,#6937,
'Flat Washer - M8:8');
#175=NEXT_ASSEMBLY_USAGE_OCCURRENCE('Cap Screw - M8x30:8',
'Cap Screw - M8x30:8','Cap Screw - M8x30:8',#6924,#6938,
'Cap Screw - M8x30:8');
#176=NEXT_ASSEMBLY_USAGE_OCCURRENCE('Flat Washer - M8:9',
'Flat Washer - M8:9','Flat Washer - M8:9',#6924,#6937,
'Flat Washer - M8:9');
#177=NEXT_ASSEMBLY_USAGE_OCCURRENCE('Cap Screw - M8x30:9',
'Cap Screw - M8x30:9','Cap Screw - M8x30:9',#6924,#6938,
'Cap Screw - M8x30:9');
#178=NEXT_ASSEMBLY_USAGE_OCCURRENCE('Revolving handle:1',
'Revolving handle:1','Revolving handle:1',#6941,#6942,
'Revolving handle:1');
#179=NEXT_ASSEMBLY_USAGE_OCCURRENCE('Handwheel shaft:1',
'Handwheel shaft:1','Handwheel shaft:1',#6939,#6940,'Handwheel shaft:1');
#180=NEXT_ASSEMBLY_USAGE_OCCURRENCE(
'Handwheel - 100 mm Diameter, 12 mm Bore:2',
'Handwheel - 100 mm Diameter, 12 mm Bore:2',
'Handwheel - 100 mm Diameter, 12 mm Bore:2',#6939,#6941,
'Handwheel - 100 mm Diameter, 12 mm Bore:2');
#181=NEXT_ASSEMBLY_USAGE_OCCURRENCE('Parallel Key - 4x4x20:2',
'Parallel Key - 4x4x20:2','Parallel Key - 4x4x20:2',#6939,#6943,
'Parallel Key - 4x4x20:2');
#182=NEXT_ASSEMBLY_USAGE_OCCURRENCE('Socket Set Screw - M6x8:2',
'Socket Set Screw - M6x8:2','Socket Set Screw - M6x8:2',#6939,#6944,
'Socket Set Screw - M6x8:2');
#183=NEXT_ASSEMBLY_USAGE_OCCURRENCE('Shaft Collar - 12 mm Bore:2',
'Shaft Collar - 12 mm Bore:2','Shaft Collar - 12 mm Bore:2',#6939,#6945,
'Shaft Collar - 12 mm Bore:2');
#184=NEXT_ASSEMBLY_USAGE_OCCURRENCE('Socket Set Screw - M5x8:2',
'Socket Set Screw - M5x8:2','Socket Set Screw - M5x8:2',#6939,#6946,
'Socket Set Screw - M5x8:2');
#185=NEXT_ASSEMBLY_USAGE_OCCURRENCE('Shaft Collar - 12 mm Bore:3',
'Shaft Collar - 12 mm Bore:3','Shaft Collar - 12 mm Bore:3',#6939,#6945,
'Shaft Collar - 12 mm Bore:3');
#186=NEXT_ASSEMBLY_USAGE_OCCURRENCE('Socket Set Screw - M5x8:3',
'Socket Set Screw - M5x8:3','Socket Set Screw - M5x8:3',#6939,#6946,
'Socket Set Screw - M5x8:3');
#187=NEXT_ASSEMBLY_USAGE_OCCURRENCE('Flanged bearing frame:1',
'Flanged bearing frame:1','Flanged bearing frame:1',#6923,#6924,
'Flanged bearing frame:1');
#188=NEXT_ASSEMBLY_USAGE_OCCURRENCE('Handwheel shaft and collars:1',
'Handwheel shaft and collars:1','Handwheel shaft and collars:1',#6923,#6939,
'Handwheel shaft and collars:1');
#189=B_SPLINE_CURVE_WITH_KNOTS('',3,(#5317,#5318,#5319,#5320,#5321,#5322,
#5323,#5324,#5325,#5326),.UNSPECIFIED.,.F.,.F.,(4,2,2,2,4),(1.13193471301885,
1.22626174930539,1.32058878559194,1.41491753480854,1.50924628402513),
 .UNSPECIFIED.);
#190=B_SPLINE_CURVE_WITH_KNOTS('',3,(#5328,#5329,#5330,#5331,#5332,#5333,
#5334,#5335,#5336,#5337,#5338,#5339,#5340,#5341,#5342,#5343,#5344,#5345),
 .UNSPECIFIED.,.F.,.F.,(4,2,2,2,2,2,2,2,4),(0.377311571006283,0.471638607292829,
0.565965643579376,0.66029439279597,0.754623142012565,0.84895189122916,0.943280640445754,
1.0376076767323,1.13193471301885),.UNSPECIFIED.);
#191=B_SPLINE_CURVE_WITH_KNOTS('',3,(#5346,#5347,#5348,#5349,#5350,#5351,
#5352,#5353,#5354,#5355),.UNSPECIFIED.,.F.,.F.,(4,2,2,2,4),(1.50924628402513,
1.60357503324173,1.69790378245832,1.79223081874487,1.88655785503141),
 .UNSPECIFIED.);
#192=B_SPLINE_CURVE_WITH_KNOTS('',3,(#5358,#5359,#5360,#5361,#5362,#5363,
#5364,#5365,#5366,#5367,#5368,#5369,#5370,#5371,#5372,#5373,#5374,#5375,
#5376,#5377,#5378,#5379,#5380,#5381,#5382,#5383,#5384,#5385,#5386,#5387,
#5388,#5389,#5390,#5391),.UNSPECIFIED.,.T.,.F.,(4,2,2,2,2,2,2,2,2,2,2,2,
2,2,2,2,4),(0.,0.0955080856649705,0.191016171329941,0.286408845249646,0.38180151916935,
0.477194193089055,0.572586867008759,0.66809495267373,0.763603038338701,
0.859111124003671,0.954619209668642,1.05001188358835,1.14540455750805,1.24079723142776,
1.33618990534746,1.43169799101243,1.5272060766774),.UNSPECIFIED.);
#193=B_SPLINE_CURVE_WITH_KNOTS('',3,(#5394,#5395,#5396,#5397,#5398,#5399,
#5400,#5401,#5402,#5403,#5404,#5405,#5406,#5407,#5408,#5409,#5410,#5411,
#5412,#5413,#5414,#5415,#5416,#5417,#5418,#5419,#5420,#5421,#5422,#5423,
#5424,#5425,#5426,#5427),.UNSPECIFIED.,.T.,.F.,(4,2,2,2,2,2,2,2,2,2,2,2,
2,2,2,2,4),(0.,0.0955080856649706,0.191016171329941,0.286408845249646,0.381801519169351,
0.477194193089055,0.57258686700876,0.668094952673731,0.763603038338701,
0.859111124003672,0.954619209668642,1.05001188358835,1.14540455750805,1.24079723142776,
1.33618990534746,1.43169799101243,1.5272060766774),.UNSPECIFIED.);
#194=B_SPLINE_CURVE_WITH_KNOTS('',3,(#5431,#5432,#5433,#5434,#5435,#5436,
#5437,#5438,#5439,#5440),.UNSPECIFIED.,.F.,.F.,(4,2,2,2,4),(1.13193471301885,
1.22626174930539,1.32058878559194,1.41491753480854,1.50924628402513),
 .UNSPECIFIED.);
#195=B_SPLINE_CURVE_WITH_KNOTS('',3,(#5442,#5443,#5444,#5445,#5446,#5447,
#5448,#5449,#5450,#5451,#5452,#5453,#5454,#5455,#5456,#5457,#5458,#5459),
 .UNSPECIFIED.,.F.,.F.,(4,2,2,2,2,2,2,2,4),(0.377311571006283,0.47163860729283,
0.565965643579376,0.660294392795971,0.754623142012565,0.84895189122916,
0.943280640445755,1.0376076767323,1.13193471301885),.UNSPECIFIED.);
#196=B_SPLINE_CURVE_WITH_KNOTS('',3,(#5460,#5461,#5462,#5463,#5464,#5465,
#5466,#5467,#5468,#5469),.UNSPECIFIED.,.F.,.F.,(4,2,2,2,4),(1.50924628402513,
1.60357503324173,1.69790378245832,1.79223081874487,1.88655785503141),
 .UNSPECIFIED.);
#197=B_SPLINE_CURVE_WITH_KNOTS('',3,(#5478,#5479,#5480,#5481,#5482,#5483,
#5484,#5485,#5486,#5487,#5488,#5489,#5490,#5491,#5492,#5493,#5494,#5495),
 .UNSPECIFIED.,.F.,.F.,(4,2,2,2,2,2,2,2,4),(0.377311571006282,0.471638607292829,
0.565965643579376,0.660294392795971,0.754623142012565,0.84895189122916,
0.943280640445754,1.0376076767323,1.13193471301885),.UNSPECIFIED.);
#198=B_SPLINE_CURVE_WITH_KNOTS('',3,(#5497,#5498,#5499,#5500,#5501,#5502,
#5503,#5504,#5505,#5506),.UNSPECIFIED.,.F.,.F.,(4,2,2,2,4),(1.13193471301885,
1.22626174930539,1.32058878559194,1.41491753480854,1.50924628402513),
 .UNSPECIFIED.);
#199=B_SPLINE_CURVE_WITH_KNOTS('',3,(#5507,#5508,#5509,#5510,#5511,#5512,
#5513,#5514,#5515,#5516),.UNSPECIFIED.,.F.,.F.,(4,2,2,2,4),(1.50924628402513,
1.60357503324172,1.69790378245832,1.79223081874487,1.88655785503141),
 .UNSPECIFIED.);
#200=B_SPLINE_CURVE_WITH_KNOTS('',3,(#5519,#5520,#5521,#5522,#5523,#5524,
#5525,#5526,#5527,#5528,#5529,#5530,#5531,#5532,#5533,#5534,#5535,#5536),
 .UNSPECIFIED.,.F.,.F.,(4,2,2,2,2,2,2,2,4),(0.377311571006283,0.47163860729283,
0.565965643579376,0.660294392795971,0.754623142012565,0.84895189122916,
0.943280640445754,1.0376076767323,1.13193471301885),.UNSPECIFIED.);
#201=B_SPLINE_CURVE_WITH_KNOTS('',3,(#5538,#5539,#5540,#5541,#5542,#5543,
#5544,#5545,#5546,#5547),.UNSPECIFIED.,.F.,.F.,(4,2,2,2,4),(1.13193471301885,
1.22626174930539,1.32058878559194,1.41491753480854,1.50924628402513),
 .UNSPECIFIED.);
#202=B_SPLINE_CURVE_WITH_KNOTS('',3,(#5548,#5549,#5550,#5551,#5552,#5553,
#5554,#5555,#5556,#5557),.UNSPECIFIED.,.F.,.F.,(4,2,2,2,4),(1.50924628402513,
1.60357503324173,1.69790378245832,1.79223081874487,1.88655785503141),
 .UNSPECIFIED.);
#203=B_SPLINE_CURVE_WITH_KNOTS('',3,(#5560,#5561,#5562,#5563,#5564,#5565,
#5566,#5567,#5568,#5569,#5570,#5571,#5572,#5573,#5574,#5575,#5576,#5577),
 .UNSPECIFIED.,.F.,.F.,(4,2,2,2,2,2,2,2,4),(0.377311571006282,0.471638607292829,
0.565965643579376,0.66029439279597,0.754623142012565,0.84895189122916,0.943280640445754,
1.0376076767323,1.13193471301885),.UNSPECIFIED.);
#204=B_SPLINE_CURVE_WITH_KNOTS('',3,(#5579,#5580,#5581,#5582,#5583,#5584,
#5585,#5586,#5587,#5588),.UNSPECIFIED.,.F.,.F.,(4,2,2,2,4),(1.13193471301885,
1.22626174930539,1.32058878559194,1.41491753480854,1.50924628402513),
 .UNSPECIFIED.);
#205=B_SPLINE_CURVE_WITH_KNOTS('',3,(#5589,#5590,#5591,#5592,#5593,#5594,
#5595,#5596,#5597,#5598),.UNSPECIFIED.,.F.,.F.,(4,2,2,2,4),(1.50924628402513,
1.60357503324172,1.69790378245832,1.79223081874487,1.88655785503141),
 .UNSPECIFIED.);
#206=B_SPLINE_CURVE_WITH_KNOTS('',3,(#5601,#5602,#5603,#5604,#5605,#5606,
#5607,#5608,#5609,#5610,#5611,#5612,#5613,#5614,#5615,#5616,#5617,#5618),
 .UNSPECIFIED.,.F.,.F.,(4,2,2,2,2,2,2,2,4),(0.377311571006283,0.471638607292829,
0.565965643579376,0.660294392795971,0.754623142012565,0.84895189122916,
0.943280640445755,1.0376076767323,1.13193471301885),.UNSPECIFIED.);
#207=B_SPLINE_CURVE_WITH_KNOTS('',3,(#5620,#5621,#5622,#5623,#5624,#5625,
#5626,#5627,#5628,#5629),.UNSPECIFIED.,.F.,.F.,(4,2,2,2,4),(1.13193471301885,
1.22626174930539,1.32058878559194,1.41491753480854,1.50924628402513),
 .UNSPECIFIED.);
#208=B_SPLINE_CURVE_WITH_KNOTS('',3,(#5630,#5631,#5632,#5633,#5634,#5635,
#5636,#5637,#5638,#5639),.UNSPECIFIED.,.F.,.F.,(4,2,2,2,4),(1.50924628402513,
1.60357503324172,1.69790378245832,1.79223081874487,1.88655785503141),
 .UNSPECIFIED.);
#209=B_SPLINE_CURVE_WITH_KNOTS('',3,(#5643,#5644,#5645,#5646,#5647,#5648,
#5649,#5650,#5651,#5652,#5653,#5654,#5655,#5656,#5657,#5658,#5659,#5660,
#5661,#5662,#5663,#5664,#5665,#5666,#5667,#5668,#5669,#5670,#5671,#5672,
#5673,#5674,#5675,#5676),.UNSPECIFIED.,.T.,.F.,(4,2,2,2,2,2,2,2,2,2,2,2,
2,2,2,2,4),(0.,0.0955080856649705,0.191016171329941,0.286408845249646,0.38180151916935,
0.477194193089055,0.572586867008759,0.66809495267373,0.7636030383387,0.859111124003671,
0.954619209668642,1.05001188358835,1.14540455750805,1.24079723142776,1.33618990534746,
1.43169799101243,1.5272060766774),.UNSPECIFIED.);
#210=B_SPLINE_CURVE_WITH_KNOTS('',3,(#5679,#5680,#5681,#5682,#5683,#5684,
#5685,#5686,#5687,#5688,#5689,#5690,#5691,#5692,#5693,#5694,#5695,#5696,
#5697,#5698,#5699,#5700,#5701,#5702,#5703,#5704,#5705,#5706,#5707,#5708,
#5709,#5710,#5711,#5712),.UNSPECIFIED.,.T.,.F.,(4,2,2,2,2,2,2,2,2,2,2,2,
2,2,2,2,4),(0.,0.0955080856649706,0.191016171329941,0.286408845249646,0.381801519169351,
0.477194193089055,0.57258686700876,0.668094952673731,0.763603038338701,
0.859111124003672,0.954619209668642,1.05001188358835,1.14540455750805,1.24079723142776,
1.33618990534746,1.43169799101243,1.5272060766774),.UNSPECIFIED.);
#211=B_SPLINE_CURVE_WITH_KNOTS('',3,(#5717,#5718,#5719,#5720,#5721,#5722,
#5723,#5724,#5725,#5726,#5727,#5728,#5729,#5730,#5731,#5732,#5733,#5734,
#5735,#5736,#5737,#5738,#5739,#5740,#5741,#5742,#5743,#5744,#5745,#5746,
#5747,#5748,#5749,#5750),.UNSPECIFIED.,.T.,.F.,(4,2,2,2,2,2,2,2,2,2,2,2,
2,2,2,2,4),(0.,0.0955080856649705,0.191016171329941,0.286408845249646,0.38180151916935,
0.477194193089055,0.572586867008759,0.66809495267373,0.7636030383387,0.859111124003671,
0.954619209668642,1.05001188358835,1.14540455750805,1.24079723142776,1.33618990534746,
1.43169799101243,1.5272060766774),.UNSPECIFIED.);
#212=B_SPLINE_CURVE_WITH_KNOTS('',3,(#5753,#5754,#5755,#5756,#5757,#5758,
#5759,#5760,#5761,#5762,#5763,#5764,#5765,#5766,#5767,#5768,#5769,#5770,
#5771,#5772,#5773,#5774,#5775,#5776,#5777,#5778,#5779,#5780,#5781,#5782,
#5783,#5784,#5785,#5786),.UNSPECIFIED.,.T.,.F.,(4,2,2,2,2,2,2,2,2,2,2,2,
2,2,2,2,4),(0.,0.0955080856649706,0.191016171329941,0.286408845249646,0.381801519169351,
0.477194193089055,0.57258686700876,0.668094952673731,0.763603038338701,
0.859111124003672,0.954619209668642,1.05001188358835,1.14540455750805,1.24079723142776,
1.33618990534746,1.43169799101243,1.5272060766774),.UNSPECIFIED.);
#213=B_SPLINE_CURVE_WITH_KNOTS('',3,(#5976,#5977,#5978,#5979,#5980,#5981,
#5982,#5983,#5984,#5985,#5986,#5987,#5988,#5989,#5990,#5991),
 .UNSPECIFIED.,.F.,.F.,(4,2,2,2,2,2,2,4),(-2.59552719332688,-2.57866585978924,
-2.54045071895435,-2.48749500888924,-2.3744647112323,-2.21556033801692,
-2.06580308432295,-1.95647920002804),.UNSPECIFIED.);
#214=B_SPLINE_CURVE_WITH_KNOTS('',3,(#5992,#5993,#5994,#5995,#5996,#5997,
#5998,#5999,#6000,#6001,#6002,#6003,#6004,#6005,#6006,#6007,#6008,#6009,
#6010,#6011,#6012,#6013,#6014,#6015,#6016,#6017,#6018,#6019,#6020,#6021,
#6022,#6023,#6024,#6025,#6026,#6027,#6028,#6029,#6030,#6031),
 .UNSPECIFIED.,.F.,.F.,(4,2,2,2,2,2,2,2,2,2,2,2,2,2,2,2,2,2,2,4),(-1.95647920002804,
-1.94940399731571,-1.82274564275395,-1.66864682416849,-1.54169125534598,
-1.43387376529483,-1.38209306412146,-1.34424705617005,-1.30493332486279,
-1.2460037370214,-1.10178537420969,-0.937426671253584,-0.78794048589305,
-0.665122735561945,-0.534841035694231,-0.375845726164312,-0.235011648675127,
-0.128548815843694,-0.0452999297674013,0.),.UNSPECIFIED.);
#215=B_SPLINE_CURVE_WITH_KNOTS('',3,(#6035,#6036,#6037,#6038,#6039,#6040,
#6041,#6042,#6043,#6044,#6045,#6046,#6047,#6048,#6049,#6050,#6051,#6052,
#6053,#6054,#6055,#6056,#6057,#6058,#6059,#6060,#6061,#6062,#6063,#6064,
#6065,#6066,#6067,#6068,#6069,#6070,#6071,#6072,#6073,#6074),
 .UNSPECIFIED.,.F.,.F.,(4,2,2,2,2,2,2,2,2,2,2,2,2,2,2,2,2,2,2,4),(-2.54361034519536,
-2.54253046486639,-2.4968571438888,-2.41437075183371,-2.26714492660274,
-2.09453621901679,-1.96116992397976,-1.84022994403498,-1.7037233477047,
-1.55334846612811,-1.42769894285765,-1.31373188966584,-1.26191388559973,
-1.22542262952322,-1.18873619849312,-1.1358415785305,-1.01347695720179,
-0.85748048653537,-0.726532050447263,-0.647957499864814),.UNSPECIFIED.);
#216=B_SPLINE_CURVE_WITH_KNOTS('',3,(#6075,#6076,#6077,#6078,#6079,#6080,
#6081,#6082,#6083,#6084,#6085,#6086,#6087,#6088,#6089,#6090),
 .UNSPECIFIED.,.F.,.F.,(4,2,2,2,2,2,2,4),(-0.647957499864814,-0.616035464948488,
-0.481588413072267,-0.322224684302864,-0.16030015410164,-0.0820369314872885,
-0.0377273936823807,0.),.UNSPECIFIED.);
#217=B_SPLINE_CURVE_WITH_KNOTS('',3,(#6094,#6095,#6096,#6097,#6098,#6099,
#6100,#6101,#6102,#6103,#6104,#6105,#6106,#6107,#6108,#6109,#6110,#6111),
 .UNSPECIFIED.,.F.,.F.,(4,2,2,2,2,2,2,2,4),(0.,0.0961983484640422,0.192396696928084,
0.28847519841324,0.384553699898396,0.480632201383552,0.576710702868707,
0.672909051332749,0.769107399796792),.UNSPECIFIED.);
#218=B_SPLINE_CURVE_WITH_KNOTS('',3,(#6112,#6113,#6114,#6115,#6116,#6117,
#6118,#6119,#6120,#6121,#6122,#6123,#6124,#6125,#6126,#6127,#6128,#6129),
 .UNSPECIFIED.,.F.,.F.,(4,2,2,2,2,2,2,2,4),(0.769107399796792,0.865305748260834,
0.961504096724876,1.05758259821003,1.15366109969519,1.24973960118034,1.3458181026655,
1.44201645112954,1.53821479959358),.UNSPECIFIED.);
#219=B_SPLINE_CURVE_WITH_KNOTS('',3,(#6133,#6134,#6135,#6136,#6137,#6138,
#6139,#6140,#6141,#6142),.UNSPECIFIED.,.F.,.F.,(4,2,2,2,4),(0.380002694880465,
0.475002363724097,0.570002032567729,0.66500371116433,0.760005389760931),
 .UNSPECIFIED.);
#220=B_SPLINE_CURVE_WITH_KNOTS('',3,(#6144,#6145,#6146,#6147,#6148,#6149,
#6150,#6151,#6152,#6153),.UNSPECIFIED.,.F.,.F.,(4,2,2,2,4),(0.,0.0950016785966008,
0.190003357193202,0.285003026036833,0.380002694880465),.UNSPECIFIED.);
#221=B_SPLINE_CURVE_WITH_KNOTS('',3,(#6155,#6156,#6157,#6158,#6159,#6160,
#6161,#6162,#6163,#6164),.UNSPECIFIED.,.F.,.F.,(4,2,2,2,4),(1.1400080846414,
1.23500775348503,1.33000742232866,1.42500910092526,1.52001077952186),
 .UNSPECIFIED.);
#222=B_SPLINE_CURVE_WITH_KNOTS('',3,(#6165,#6166,#6167,#6168,#6169,#6170,
#6171,#6172,#6173,#6174),.UNSPECIFIED.,.F.,.F.,(4,2,2,2,4),(0.760005389760931,
0.855007068357531,0.950008746954132,1.04500841579776,1.1400080846414),
 .UNSPECIFIED.);
#223=B_SPLINE_CURVE_WITH_KNOTS('',3,(#6205,#6206,#6207,#6208,#6209,#6210,
#6211,#6212,#6213,#6214,#6215,#6216,#6217,#6218),.UNSPECIFIED.,.F.,.F.,
(4,2,2,2,2,2,4),(-2.54850355944817,-2.47147966009112,-2.35116278368337,
-2.17207383157567,-2.03290678540533,-1.91210887606818,-1.90533893688978),
 .UNSPECIFIED.);
#224=B_SPLINE_CURVE_WITH_KNOTS('',3,(#6220,#6221,#6222,#6223,#6224,#6225,
#6226,#6227,#6228,#6229,#6230,#6231),.UNSPECIFIED.,.F.,.F.,(4,2,2,2,2,4),
(-0.637276313354589,-0.528249228810808,-0.380873908763749,-0.202177241884586,
-0.0799314225938296,0.),.UNSPECIFIED.);
#225=B_SPLINE_CURVE_WITH_KNOTS('',3,(#6234,#6235,#6236,#6237,#6238,#6239,
#6240,#6241,#6242,#6243,#6244,#6245,#6246,#6247,#6248,#6249,#6250,#6251,
#6252,#6253,#6254,#6255,#6256,#6257,#6258,#6259,#6260,#6261,#6262,#6263,
#6264,#6265,#6266,#6267),.UNSPECIFIED.,.T.,.F.,(4,2,2,2,2,2,2,2,2,2,2,2,
2,2,2,2,4),(0.,0.151379292814069,0.302758585628139,0.454116712920023,0.605474840211907,
0.756832967503791,0.908191094795676,1.05957038760974,1.21094968042381,1.36232897323788,
1.51370826605195,1.66506639334384,1.81642452063572,1.96778264792761,2.11914077521949,
2.27052006803356,2.42189936084763),.UNSPECIFIED.);
#226=B_SPLINE_CURVE_WITH_KNOTS('',3,(#6268,#6269,#6270,#6271,#6272,#6273,
#6274,#6275,#6276,#6277,#6278,#6279,#6280,#6281,#6282,#6283,#6284,#6285,
#6286,#6287,#6288,#6289,#6290,#6291),.UNSPECIFIED.,.F.,.F.,(4,2,2,2,2,2,
2,2,2,2,2,4),(-1.90533893688978,-1.78642522838365,-1.63371704918402,-1.47883830887698,
-1.3527241089287,-1.27308869766128,-1.19599240460016,-1.08166165023207,
-0.90752604130311,-0.769338857038376,-0.650696729228082,-0.637276313354589),
 .UNSPECIFIED.);
#227=B_SPLINE_CURVE_WITH_KNOTS('',3,(#6295,#6296,#6297,#6298,#6299,#6300,
#6301,#6302,#6303,#6304,#6305,#6306,#6307,#6308),.UNSPECIFIED.,.F.,.F.,
(4,2,2,2,2,2,4),(-2.5485035594474,-2.47147966009035,-2.35116278368264,-2.17207383157505,
-2.0329067854048,-1.91210887606772,-1.90533893688933),.UNSPECIFIED.);
#228=B_SPLINE_CURVE_WITH_KNOTS('',3,(#6310,#6311,#6312,#6313,#6314,#6315,
#6316,#6317,#6318,#6319,#6320,#6321),.UNSPECIFIED.,.F.,.F.,(4,2,2,2,2,4),
(-0.637276313354588,-0.528249228810783,-0.380873908763716,-0.202177241884562,
-0.0799314225938254,0.),.UNSPECIFIED.);
#229=B_SPLINE_CURVE_WITH_KNOTS('',3,(#6324,#6325,#6326,#6327,#6328,#6329,
#6330,#6331,#6332,#6333,#6334,#6335,#6336,#6337,#6338,#6339,#6340,#6341,
#6342,#6343,#6344,#6345,#6346,#6347,#6348,#6349,#6350,#6351,#6352,#6353,
#6354,#6355,#6356,#6357),.UNSPECIFIED.,.T.,.F.,(4,2,2,2,2,2,2,2,2,2,2,2,
2,2,2,2,4),(0.,0.151379292814069,0.302758585628139,0.454116712920023,0.605474840211907,
0.756832967503791,0.908191094795675,1.05957038760974,1.21094968042381,1.36232897323788,
1.51370826605195,1.66506639334384,1.81642452063572,1.9677826479276,2.11914077521949,
2.27052006803356,2.42189936084763),.UNSPECIFIED.);
#230=B_SPLINE_CURVE_WITH_KNOTS('',3,(#6358,#6359,#6360,#6361,#6362,#6363,
#6364,#6365,#6366,#6367,#6368,#6369,#6370,#6371,#6372,#6373,#6374,#6375,
#6376,#6377,#6378,#6379,#6380,#6381),.UNSPECIFIED.,.F.,.F.,(4,2,2,2,2,2,
2,2,2,2,2,4),(-1.90533893688933,-1.78642522838326,-1.63371704918372,-1.47883830887675,
-1.35272410892854,-1.27308869766117,-1.1959924046001,-1.08166165023206,
-0.907526041303146,-0.7693388570384,-0.65069672922808,-0.637276313354588),
 .UNSPECIFIED.);
#231=B_SPLINE_CURVE_WITH_KNOTS('',3,(#6385,#6386,#6387,#6388,#6389,#6390,
#6391,#6392,#6393,#6394,#6395,#6396),.UNSPECIFIED.,.F.,.F.,(4,2,2,2,2,4),
(-2.61916424636074,-2.54165598774645,-2.39715438567385,-2.22985321946239,
-2.07412217165227,-1.96431456403181),.UNSPECIFIED.);
#232=B_SPLINE_CURVE_WITH_KNOTS('',3,(#6398,#6399,#6400,#6401,#6402,#6403,
#6404,#6405,#6406,#6407,#6408,#6409),.UNSPECIFIED.,.F.,.F.,(4,2,2,2,2,4),
(-0.649106074577762,-0.568991182312238,-0.428137419269516,-0.24870582271537,
-0.112671421215055,0.),.UNSPECIFIED.);
#233=B_SPLINE_CURVE_WITH_KNOTS('',3,(#6412,#6413,#6414,#6415,#6416,#6417,
#6418,#6419,#6420,#6421,#6422,#6423,#6424,#6425,#6426,#6427,#6428,#6429,
#6430,#6431,#6432,#6433,#6434,#6435,#6436,#6437,#6438,#6439,#6440,#6441,
#6442,#6443,#6444,#6445),.UNSPECIFIED.,.T.,.F.,(4,2,2,2,2,2,2,2,2,2,2,2,
2,2,2,2,4),(0.,0.151379292814069,0.302758585628139,0.454116712920023,0.605474840211907,
0.756832967503791,0.908191094795675,1.05957038760974,1.21094968042381,1.36232897323788,
1.51370826605195,1.66506639334384,1.81642452063572,1.96778264792761,2.11914077521949,
2.27052006803356,2.42189936084763),.UNSPECIFIED.);
#234=B_SPLINE_CURVE_WITH_KNOTS('',3,(#6446,#6447,#6448,#6449,#6450,#6451,
#6452,#6453,#6454,#6455,#6456,#6457,#6458,#6459,#6460,#6461,#6462,#6463,
#6464,#6465,#6466,#6467,#6468,#6469),.UNSPECIFIED.,.F.,.F.,(4,2,2,2,2,2,
2,2,2,2,2,4),(-1.96431456403181,-1.95510446892338,-1.83271225668806,-1.67410879488211,
-1.50389075900942,-1.37768596650605,-1.25930643549399,-1.12433269575576,
-0.949014691445703,-0.810038710964932,-0.682802605332806,-0.649106074577762),
 .UNSPECIFIED.);
#235=B_SPLINE_CURVE_WITH_KNOTS('',3,(#6600,#6601,#6602,#6603,#6604,#6605,
#6606,#6607,#6608,#6609,#6610,#6611,#6612,#6613,#6614,#6615,#6616,#6617,
#6618,#6619,#6620,#6621,#6622,#6623,#6624,#6625,#6626,#6627,#6628,#6629,
#6630,#6631,#6632,#6633),.UNSPECIFIED.,.T.,.F.,(4,2,2,2,2,2,2,2,2,2,2,2,
2,2,2,2,4),(0.,0.0805240527913139,0.161048105582628,0.241524630728584,0.322001155874541,
0.402477681020498,0.482954206166455,0.563478258957768,0.644002311749082,
0.724526364540396,0.80505041733171,0.885526942477667,0.966003467623624,
1.04647999276958,1.12695651791554,1.20748057070685,1.28800462349816),
 .UNSPECIFIED.);
#236=B_SPLINE_CURVE_WITH_KNOTS('',3,(#6636,#6637,#6638,#6639,#6640,#6641,
#6642,#6643,#6644,#6645,#6646,#6647,#6648,#6649,#6650,#6651,#6652,#6653,
#6654,#6655,#6656,#6657,#6658,#6659,#6660,#6661,#6662,#6663,#6664,#6665,
#6666,#6667,#6668,#6669),.UNSPECIFIED.,.T.,.F.,(4,2,2,2,2,2,2,2,2,2,2,2,
2,2,2,2,4),(0.,0.0799614062161292,0.159922812432258,0.239880387792505,0.319837963152752,
0.399795538512999,0.479753113873245,0.559714520089374,0.639675926305503,
0.719637332521632,0.799598738737761,0.879556314098008,0.959513889458255,
1.0394714648185,1.11942904017875,1.19939044639488,1.27935185261101),
 .UNSPECIFIED.);
#237=SPHERICAL_SURFACE('',#3681,2.35);
#238=SPHERICAL_SURFACE('',#3719,2.35);
#239=SHAPE_REPRESENTATION_RELATIONSHIP('SRR','None',#6900,#259);
#240=SHAPE_REPRESENTATION_RELATIONSHIP('SRR','None',#6901,#260);
#241=SHAPE_REPRESENTATION_RELATIONSHIP('SRR','None',#6902,#261);
#242=SHAPE_REPRESENTATION_RELATIONSHIP('SRR','None',#6903,#262);
#243=SHAPE_REPRESENTATION_RELATIONSHIP('SRR','None',#6904,#263);
#244=SHAPE_REPRESENTATION_RELATIONSHIP('SRR','None',#6905,#264);
#245=SHAPE_REPRESENTATION_RELATIONSHIP('SRR','None',#6906,#265);
#246=SHAPE_REPRESENTATION_RELATIONSHIP('SRR','None',#6907,#266);
#247=SHAPE_REPRESENTATION_RELATIONSHIP('SRR','None',#6908,#267);
#248=SHAPE_REPRESENTATION_RELATIONSHIP('SRR','None',#6910,#268);
#249=SHAPE_REPRESENTATION_RELATIONSHIP('SRR','None',#6911,#269);
#250=SHAPE_REPRESENTATION_RELATIONSHIP('SRR','None',#6912,#270);
#251=SHAPE_REPRESENTATION_RELATIONSHIP('SRR','None',#6913,#271);
#252=SHAPE_REPRESENTATION_RELATIONSHIP('SRR','None',#6915,#272);
#253=SHAPE_REPRESENTATION_RELATIONSHIP('SRR','None',#6917,#273);
#254=SHAPE_REPRESENTATION_RELATIONSHIP('SRR','None',#6916,#274);
#255=SHAPE_REPRESENTATION_RELATIONSHIP('SRR','None',#6918,#275);
#256=SHAPE_REPRESENTATION_RELATIONSHIP('SRR','None',#6919,#276);
#257=SHAPE_REPRESENTATION_RELATIONSHIP('SRR','None',#6920,#277);
#258=SHAPE_REPRESENTATION_RELATIONSHIP('SRR','None',#6921,#278);
#259=ADVANCED_BREP_SHAPE_REPRESENTATION('',(#300),#6783);
#260=ADVANCED_BREP_SHAPE_REPRESENTATION('',(#301),#6784);
#261=ADVANCED_BREP_SHAPE_REPRESENTATION('',(#302),#6785);
#262=ADVANCED_BREP_SHAPE_REPRESENTATION('',(#303),#6786);
#263=ADVANCED_BREP_SHAPE_REPRESENTATION('',(#304),#6787);
#264=ADVANCED_BREP_SHAPE_REPRESENTATION('',(#305),#6788);
#265=ADVANCED_BREP_SHAPE_REPRESENTATION('',(#306),#6789);
#266=ADVANCED_BREP_SHAPE_REPRESENTATION('',(#307),#6790);
#267=ADVANCED_BREP_SHAPE_REPRESENTATION('',(#308),#6791);
#268=ADVANCED_BREP_SHAPE_REPRESENTATION('',(#309),#6793);
#269=ADVANCED_BREP_SHAPE_REPRESENTATION('',(#310,#311),#6794);
#270=ADVANCED_BREP_SHAPE_REPRESENTATION('',(#312),#6795);
#271=ADVANCED_BREP_SHAPE_REPRESENTATION('',(#28),#6796);
#272=ADVANCED_BREP_SHAPE_REPRESENTATION('',(#313),#6798);
#273=ADVANCED_BREP_SHAPE_REPRESENTATION('',(#314),#6800);
#274=ADVANCED_BREP_SHAPE_REPRESENTATION('',(#315),#6799);
#275=ADVANCED_BREP_SHAPE_REPRESENTATION('',(#316),#6801);
#276=ADVANCED_BREP_SHAPE_REPRESENTATION('',(#317),#6802);
#277=ADVANCED_BREP_SHAPE_REPRESENTATION('',(#318),#6803);
#278=ADVANCED_BREP_SHAPE_REPRESENTATION('',(#319),#6804);
#279=STYLED_ITEM('',(#7091),#300);
#280=STYLED_ITEM('',(#7098),#301);
#281=STYLED_ITEM('',(#7098),#302);
#282=STYLED_ITEM('',(#7098),#303);
#283=STYLED_ITEM('',(#7098),#304);
#284=STYLED_ITEM('',(#7098),#305);
#285=STYLED_ITEM('',(#7098),#306);
#286=STYLED_ITEM('',(#7098),#307);
#287=STYLED_ITEM('',(#7098),#308);
#288=STYLED_ITEM('',(#7070),#309);
#289=STYLED_ITEM('',(#7091),#310);
#290=STYLED_ITEM('',(#7091),#311);
#291=STYLED_ITEM('',(#7098),#312);
#292=STYLED_ITEM('',(#7098),#28);
#293=STYLED_ITEM('',(#7091),#313);
#294=STYLED_ITEM('',(#7084),#314);
#295=STYLED_ITEM('',(#7084),#315);
#296=STYLED_ITEM('',(#7091),#316);
#297=STYLED_ITEM('',(#7098),#317);
#298=STYLED_ITEM('',(#7091),#318);
#299=STYLED_ITEM('',(#7098),#319);
#300=MANIFOLD_SOLID_BREP('Body1',#3320);
#301=MANIFOLD_SOLID_BREP('Body1',#3321);
#302=MANIFOLD_SOLID_BREP('Body1',#3322);
#303=MANIFOLD_SOLID_BREP('Body1',#3323);
#304=MANIFOLD_SOLID_BREP('Body1',#3324);
#305=MANIFOLD_SOLID_BREP('Body1',#3325);
#306=MANIFOLD_SOLID_BREP('Body1',#3326);
#307=MANIFOLD_SOLID_BREP('Body1',#3327);
#308=MANIFOLD_SOLID_BREP('Body1',#3328);
#309=MANIFOLD_SOLID_BREP('Body1',#3329);
#310=MANIFOLD_SOLID_BREP('Body1',#3330);
#311=MANIFOLD_SOLID_BREP('Body2',#3331);
#312=MANIFOLD_SOLID_BREP('Body1',#3332);
#313=MANIFOLD_SOLID_BREP('Body1',#3335);
#314=MANIFOLD_SOLID_BREP('Body1',#3336);
#315=MANIFOLD_SOLID_BREP('Body1',#3337);
#316=MANIFOLD_SOLID_BREP('Body1',#3338);
#317=MANIFOLD_SOLID_BREP('Body1',#3339);
#318=MANIFOLD_SOLID_BREP('Body1',#3340);
#319=MANIFOLD_SOLID_BREP('Body1',#3341);
#320=FACE_BOUND('',#712,.T.);
#321=FACE_BOUND('',#713,.T.);
#322=FACE_BOUND('',#714,.T.);
#323=FACE_BOUND('',#715,.T.);
#324=FACE_BOUND('',#716,.T.);
#325=FACE_BOUND('',#718,.T.);
#326=FACE_BOUND('',#719,.T.);
#327=FACE_BOUND('',#720,.T.);
#328=FACE_BOUND('',#721,.T.);
#329=FACE_BOUND('',#722,.T.);
#330=FACE_BOUND('',#732,.T.);
#331=FACE_BOUND('',#733,.T.);
#332=FACE_BOUND('',#734,.T.);
#333=FACE_BOUND('',#735,.T.);
#334=FACE_BOUND('',#736,.T.);
#335=FACE_BOUND('',#738,.T.);
#336=FACE_BOUND('',#739,.T.);
#337=FACE_BOUND('',#740,.T.);
#338=FACE_BOUND('',#741,.T.);
#339=FACE_BOUND('',#742,.T.);
#340=FACE_BOUND('',#748,.T.);
#341=FACE_BOUND('',#749,.T.);
#342=FACE_BOUND('',#754,.T.);
#343=FACE_BOUND('',#756,.T.);
#344=FACE_BOUND('',#760,.T.);
#345=FACE_BOUND('',#762,.T.);
#346=FACE_BOUND('',#766,.T.);
#347=FACE_BOUND('',#768,.T.);
#348=FACE_BOUND('',#772,.T.);
#349=FACE_BOUND('',#774,.T.);
#350=FACE_BOUND('',#778,.T.);
#351=FACE_BOUND('',#780,.T.);
#352=FACE_BOUND('',#784,.T.);
#353=FACE_BOUND('',#786,.T.);
#354=FACE_BOUND('',#790,.T.);
#355=FACE_BOUND('',#792,.T.);
#356=FACE_BOUND('',#796,.T.);
#357=FACE_BOUND('',#798,.T.);
#358=FACE_BOUND('',#802,.T.);
#359=FACE_BOUND('',#803,.T.);
#360=FACE_BOUND('',#807,.T.);
#361=FACE_BOUND('',#809,.T.);
#362=FACE_BOUND('',#823,.T.);
#363=FACE_BOUND('',#824,.T.);
#364=FACE_BOUND('',#825,.T.);
#365=FACE_BOUND('',#826,.T.);
#366=FACE_BOUND('',#827,.T.);
#367=FACE_BOUND('',#829,.T.);
#368=FACE_BOUND('',#830,.T.);
#369=FACE_BOUND('',#831,.T.);
#370=FACE_BOUND('',#832,.T.);
#371=FACE_BOUND('',#833,.T.);
#372=FACE_BOUND('',#836,.T.);
#373=FACE_BOUND('',#838,.T.);
#374=FACE_BOUND('',#839,.T.);
#375=FACE_BOUND('',#841,.T.);
#376=FACE_BOUND('',#845,.T.);
#377=FACE_BOUND('',#846,.T.);
#378=FACE_BOUND('',#847,.T.);
#379=FACE_BOUND('',#848,.T.);
#380=FACE_BOUND('',#849,.T.);
#381=FACE_BOUND('',#850,.T.);
#382=FACE_BOUND('',#856,.T.);
#383=FACE_BOUND('',#858,.T.);
#384=FACE_BOUND('',#861,.T.);
#385=FACE_BOUND('',#863,.T.);
#386=FACE_BOUND('',#864,.T.);
#387=FACE_BOUND('',#865,.T.);
#388=FACE_BOUND('',#866,.T.);
#389=FACE_BOUND('',#867,.T.);
#390=FACE_BOUND('',#868,.T.);
#391=FACE_BOUND('',#872,.T.);
#392=FACE_BOUND('',#874,.T.);
#393=FACE_BOUND('',#880,.T.);
#394=FACE_BOUND('',#899,.T.);
#395=FACE_BOUND('',#906,.T.);
#396=FACE_BOUND('',#915,.T.);
#397=FACE_BOUND('',#917,.T.);
#398=FACE_BOUND('',#922,.T.);
#399=FACE_BOUND('',#924,.T.);
#400=FACE_BOUND('',#925,.T.);
#401=FACE_BOUND('',#926,.T.);
#402=FACE_BOUND('',#928,.T.);
#403=FACE_BOUND('',#929,.T.);
#404=FACE_BOUND('',#952,.T.);
#405=FACE_BOUND('',#959,.T.);
#406=FACE_BOUND('',#962,.T.);
#407=FACE_BOUND('',#965,.T.);
#408=FACE_BOUND('',#967,.T.);
#409=FACE_BOUND('',#976,.T.);
#410=PLANE('',#3570);
#411=PLANE('',#3571);
#412=PLANE('',#3572);
#413=PLANE('',#3573);
#414=PLANE('',#3574);
#415=PLANE('',#3590);
#416=PLANE('',#3591);
#417=PLANE('',#3592);
#418=PLANE('',#3593);
#419=PLANE('',#3594);
#420=PLANE('',#3595);
#421=PLANE('',#3596);
#422=PLANE('',#3597);
#423=PLANE('',#3598);
#424=PLANE('',#3599);
#425=PLANE('',#3600);
#426=PLANE('',#3608);
#427=PLANE('',#3609);
#428=PLANE('',#3617);
#429=PLANE('',#3618);
#430=PLANE('',#3626);
#431=PLANE('',#3627);
#432=PLANE('',#3635);
#433=PLANE('',#3636);
#434=PLANE('',#3644);
#435=PLANE('',#3645);
#436=PLANE('',#3653);
#437=PLANE('',#3654);
#438=PLANE('',#3662);
#439=PLANE('',#3663);
#440=PLANE('',#3671);
#441=PLANE('',#3672);
#442=PLANE('',#3689);
#443=PLANE('',#3690);
#444=PLANE('',#3703);
#445=PLANE('',#3704);
#446=PLANE('',#3705);
#447=PLANE('',#3706);
#448=PLANE('',#3707);
#449=PLANE('',#3708);
#450=PLANE('',#3709);
#451=PLANE('',#3710);
#452=PLANE('',#3711);
#453=PLANE('',#3712);
#454=PLANE('',#3717);
#455=PLANE('',#3722);
#456=PLANE('',#3732);
#457=PLANE('',#3734);
#458=PLANE('',#3738);
#459=PLANE('',#3750);
#460=PLANE('',#3751);
#461=PLANE('',#3753);
#462=PLANE('',#3761);
#463=PLANE('',#3769);
#464=PLANE('',#3770);
#465=PLANE('',#3771);
#466=PLANE('',#3772);
#467=PLANE('',#3773);
#468=PLANE('',#3774);
#469=PLANE('',#3775);
#470=PLANE('',#3776);
#471=PLANE('',#3777);
#472=PLANE('',#3807);
#473=PLANE('',#3808);
#474=PLANE('',#3810);
#475=PLANE('',#3811);
#476=PLANE('',#3812);
#477=PLANE('',#3817);
#478=PLANE('',#3818);
#479=PLANE('',#3821);
#480=PLANE('',#3827);
#481=PLANE('',#3831);
#482=PLANE('',#3834);
#483=PLANE('',#3835);
#484=PLANE('',#3836);
#485=PLANE('',#3837);
#486=PLANE('',#3845);
#487=PLANE('',#3856);
#488=PLANE('',#3860);
#489=PLANE('',#3866);
#490=PLANE('',#3867);
#491=PLANE('',#3868);
#492=PLANE('',#3871);
#493=PLANE('',#3876);
#494=PLANE('',#3877);
#495=PLANE('',#3879);
#496=PLANE('',#3880);
#497=PLANE('',#3881);
#498=PLANE('',#3882);
#499=PLANE('',#3883);
#500=PLANE('',#3884);
#501=PLANE('',#3885);
#502=PLANE('',#3886);
#503=PLANE('',#3894);
#504=PLANE('',#3897);
#505=PLANE('',#3906);
#506=PLANE('',#3910);
#507=PLANE('',#3911);
#508=PLANE('',#3912);
#509=PLANE('',#3913);
#510=PLANE('',#3914);
#511=PLANE('',#3915);
#512=PLANE('',#3916);
#513=PLANE('',#3917);
#514=PLANE('',#3925);
#515=FACE_OUTER_BOUND('',#703,.T.);
#516=FACE_OUTER_BOUND('',#704,.T.);
#517=FACE_OUTER_BOUND('',#705,.T.);
#518=FACE_OUTER_BOUND('',#706,.T.);
#519=FACE_OUTER_BOUND('',#707,.T.);
#520=FACE_OUTER_BOUND('',#708,.T.);
#521=FACE_OUTER_BOUND('',#709,.T.);
#522=FACE_OUTER_BOUND('',#710,.T.);
#523=FACE_OUTER_BOUND('',#711,.T.);
#524=FACE_OUTER_BOUND('',#717,.T.);
#525=FACE_OUTER_BOUND('',#723,.T.);
#526=FACE_OUTER_BOUND('',#724,.T.);
#527=FACE_OUTER_BOUND('',#725,.T.);
#528=FACE_OUTER_BOUND('',#726,.T.);
#529=FACE_OUTER_BOUND('',#727,.T.);
#530=FACE_OUTER_BOUND('',#728,.T.);
#531=FACE_OUTER_BOUND('',#729,.T.);
#532=FACE_OUTER_BOUND('',#730,.T.);
#533=FACE_OUTER_BOUND('',#731,.T.);
#534=FACE_OUTER_BOUND('',#737,.T.);
#535=FACE_OUTER_BOUND('',#743,.T.);
#536=FACE_OUTER_BOUND('',#744,.T.);
#537=FACE_OUTER_BOUND('',#745,.T.);
#538=FACE_OUTER_BOUND('',#746,.T.);
#539=FACE_OUTER_BOUND('',#747,.T.);
#540=FACE_OUTER_BOUND('',#750,.T.);
#541=FACE_OUTER_BOUND('',#751,.T.);
#542=FACE_OUTER_BOUND('',#752,.T.);
#543=FACE_OUTER_BOUND('',#753,.T.);
#544=FACE_OUTER_BOUND('',#755,.T.);
#545=FACE_OUTER_BOUND('',#757,.T.);
#546=FACE_OUTER_BOUND('',#758,.T.);
#547=FACE_OUTER_BOUND('',#759,.T.);
#548=FACE_OUTER_BOUND('',#761,.T.);
#549=FACE_OUTER_BOUND('',#763,.T.);
#550=FACE_OUTER_BOUND('',#764,.T.);
#551=FACE_OUTER_BOUND('',#765,.T.);
#552=FACE_OUTER_BOUND('',#767,.T.);
#553=FACE_OUTER_BOUND('',#769,.T.);
#554=FACE_OUTER_BOUND('',#770,.T.);
#555=FACE_OUTER_BOUND('',#771,.T.);
#556=FACE_OUTER_BOUND('',#773,.T.);
#557=FACE_OUTER_BOUND('',#775,.T.);
#558=FACE_OUTER_BOUND('',#776,.T.);
#559=FACE_OUTER_BOUND('',#777,.T.);
#560=FACE_OUTER_BOUND('',#779,.T.);
#561=FACE_OUTER_BOUND('',#781,.T.);
#562=FACE_OUTER_BOUND('',#782,.T.);
#563=FACE_OUTER_BOUND('',#783,.T.);
#564=FACE_OUTER_BOUND('',#785,.T.);
#565=FACE_OUTER_BOUND('',#787,.T.);
#566=FACE_OUTER_BOUND('',#788,.T.);
#567=FACE_OUTER_BOUND('',#789,.T.);
#568=FACE_OUTER_BOUND('',#791,.T.);
#569=FACE_OUTER_BOUND('',#793,.T.);
#570=FACE_OUTER_BOUND('',#794,.T.);
#571=FACE_OUTER_BOUND('',#795,.T.);
#572=FACE_OUTER_BOUND('',#797,.T.);
#573=FACE_OUTER_BOUND('',#799,.T.);
#574=FACE_OUTER_BOUND('',#800,.T.);
#575=FACE_OUTER_BOUND('',#801,.T.);
#576=FACE_OUTER_BOUND('',#804,.T.);
#577=FACE_OUTER_BOUND('',#805,.T.);
#578=FACE_OUTER_BOUND('',#806,.T.);
#579=FACE_OUTER_BOUND('',#808,.T.);
#580=FACE_OUTER_BOUND('',#810,.T.);
#581=FACE_OUTER_BOUND('',#811,.T.);
#582=FACE_OUTER_BOUND('',#812,.T.);
#583=FACE_OUTER_BOUND('',#813,.T.);
#584=FACE_OUTER_BOUND('',#814,.T.);
#585=FACE_OUTER_BOUND('',#815,.T.);
#586=FACE_OUTER_BOUND('',#816,.T.);
#587=FACE_OUTER_BOUND('',#817,.T.);
#588=FACE_OUTER_BOUND('',#818,.T.);
#589=FACE_OUTER_BOUND('',#819,.T.);
#590=FACE_OUTER_BOUND('',#820,.T.);
#591=FACE_OUTER_BOUND('',#821,.T.);
#592=FACE_OUTER_BOUND('',#822,.T.);
#593=FACE_OUTER_BOUND('',#828,.T.);
#594=FACE_OUTER_BOUND('',#834,.T.);
#595=FACE_OUTER_BOUND('',#835,.T.);
#596=FACE_OUTER_BOUND('',#837,.T.);
#597=FACE_OUTER_BOUND('',#840,.T.);
#598=FACE_OUTER_BOUND('',#842,.T.);
#599=FACE_OUTER_BOUND('',#843,.T.);
#600=FACE_OUTER_BOUND('',#844,.T.);
#601=FACE_OUTER_BOUND('',#851,.T.);
#602=FACE_OUTER_BOUND('',#852,.T.);
#603=FACE_OUTER_BOUND('',#853,.T.);
#604=FACE_OUTER_BOUND('',#854,.T.);
#605=FACE_OUTER_BOUND('',#855,.T.);
#606=FACE_OUTER_BOUND('',#857,.T.);
#607=FACE_OUTER_BOUND('',#859,.T.);
#608=FACE_OUTER_BOUND('',#860,.T.);
#609=FACE_OUTER_BOUND('',#862,.T.);
#610=FACE_OUTER_BOUND('',#869,.T.);
#611=FACE_OUTER_BOUND('',#870,.T.);
#612=FACE_OUTER_BOUND('',#871,.T.);
#613=FACE_OUTER_BOUND('',#873,.T.);
#614=FACE_OUTER_BOUND('',#875,.T.);
#615=FACE_OUTER_BOUND('',#876,.T.);
#616=FACE_OUTER_BOUND('',#877,.T.);
#617=FACE_OUTER_BOUND('',#878,.T.);
#618=FACE_OUTER_BOUND('',#879,.T.);
#619=FACE_OUTER_BOUND('',#881,.T.);
#620=FACE_OUTER_BOUND('',#882,.T.);
#621=FACE_OUTER_BOUND('',#883,.T.);
#622=FACE_OUTER_BOUND('',#884,.T.);
#623=FACE_OUTER_BOUND('',#885,.T.);
#624=FACE_OUTER_BOUND('',#886,.T.);
#625=FACE_OUTER_BOUND('',#887,.T.);
#626=FACE_OUTER_BOUND('',#888,.T.);
#627=FACE_OUTER_BOUND('',#889,.T.);
#628=FACE_OUTER_BOUND('',#890,.T.);
#629=FACE_OUTER_BOUND('',#891,.T.);
#630=FACE_OUTER_BOUND('',#892,.T.);
#631=FACE_OUTER_BOUND('',#893,.T.);
#632=FACE_OUTER_BOUND('',#894,.T.);
#633=FACE_OUTER_BOUND('',#895,.T.);
#634=FACE_OUTER_BOUND('',#896,.T.);
#635=FACE_OUTER_BOUND('',#897,.T.);
#636=FACE_OUTER_BOUND('',#898,.T.);
#637=FACE_OUTER_BOUND('',#900,.T.);
#638=FACE_OUTER_BOUND('',#901,.T.);
#639=FACE_OUTER_BOUND('',#902,.T.);
#640=FACE_OUTER_BOUND('',#903,.T.);
#641=FACE_OUTER_BOUND('',#904,.T.);
#642=FACE_OUTER_BOUND('',#905,.T.);
#643=FACE_OUTER_BOUND('',#907,.T.);
#644=FACE_OUTER_BOUND('',#908,.T.);
#645=FACE_OUTER_BOUND('',#909,.T.);
#646=FACE_OUTER_BOUND('',#910,.T.);
#647=FACE_OUTER_BOUND('',#911,.T.);
#648=FACE_OUTER_BOUND('',#912,.T.);
#649=FACE_OUTER_BOUND('',#913,.T.);
#650=FACE_OUTER_BOUND('',#914,.T.);
#651=FACE_OUTER_BOUND('',#916,.T.);
#652=FACE_OUTER_BOUND('',#918,.T.);
#653=FACE_OUTER_BOUND('',#919,.T.);
#654=FACE_OUTER_BOUND('',#920,.T.);
#655=FACE_OUTER_BOUND('',#921,.T.);
#656=FACE_OUTER_BOUND('',#923,.T.);
#657=FACE_OUTER_BOUND('',#927,.T.);
#658=FACE_OUTER_BOUND('',#930,.T.);
#659=FACE_OUTER_BOUND('',#931,.T.);
#660=FACE_OUTER_BOUND('',#932,.T.);
#661=FACE_OUTER_BOUND('',#933,.T.);
#662=FACE_OUTER_BOUND('',#934,.T.);
#663=FACE_OUTER_BOUND('',#935,.T.);
#664=FACE_OUTER_BOUND('',#936,.T.);
#665=FACE_OUTER_BOUND('',#937,.T.);
#666=FACE_OUTER_BOUND('',#938,.T.);
#667=FACE_OUTER_BOUND('',#939,.T.);
#668=FACE_OUTER_BOUND('',#940,.T.);
#669=FACE_OUTER_BOUND('',#941,.T.);
#670=FACE_OUTER_BOUND('',#942,.T.);
#671=FACE_OUTER_BOUND('',#943,.T.);
#672=FACE_OUTER_BOUND('',#944,.T.);
#673=FACE_OUTER_BOUND('',#945,.T.);
#674=FACE_OUTER_BOUND('',#946,.T.);
#675=FACE_OUTER_BOUND('',#947,.T.);
#676=FACE_OUTER_BOUND('',#948,.T.);
#677=FACE_OUTER_BOUND('',#949,.T.);
#678=FACE_OUTER_BOUND('',#950,.T.);
#679=FACE_OUTER_BOUND('',#951,.T.);
#680=FACE_OUTER_BOUND('',#953,.T.);
#681=FACE_OUTER_BOUND('',#954,.T.);
#682=FACE_OUTER_BOUND('',#955,.T.);
#683=FACE_OUTER_BOUND('',#956,.T.);
#684=FACE_OUTER_BOUND('',#957,.T.);
#685=FACE_OUTER_BOUND('',#958,.T.);
#686=FACE_OUTER_BOUND('',#960,.T.);
#687=FACE_OUTER_BOUND('',#961,.T.);
#688=FACE_OUTER_BOUND('',#963,.T.);
#689=FACE_OUTER_BOUND('',#964,.T.);
#690=FACE_OUTER_BOUND('',#966,.T.);
#691=FACE_OUTER_BOUND('',#968,.T.);
#692=FACE_OUTER_BOUND('',#969,.T.);
#693=FACE_OUTER_BOUND('',#970,.T.);
#694=FACE_OUTER_BOUND('',#971,.T.);
#695=FACE_OUTER_BOUND('',#972,.T.);
#696=FACE_OUTER_BOUND('',#973,.T.);
#697=FACE_OUTER_BOUND('',#974,.T.);
#698=FACE_OUTER_BOUND('',#975,.T.);
#699=FACE_OUTER_BOUND('',#977,.T.);
#700=FACE_OUTER_BOUND('',#978,.T.);
#701=FACE_OUTER_BOUND('',#979,.T.);
#702=FACE_OUTER_BOUND('',#980,.T.);
#703=EDGE_LOOP('',(#2251,#2252,#2253,#2254));
#704=EDGE_LOOP('',(#2255,#2256,#2257,#2258));
#705=EDGE_LOOP('',(#2259,#2260,#2261,#2262));
#706=EDGE_LOOP('',(#2263,#2264,#2265,#2266));
#707=EDGE_LOOP('',(#2267,#2268,#2269,#2270));
#708=EDGE_LOOP('',(#2271,#2272,#2273,#2274));
#709=EDGE_LOOP('',(#2275,#2276,#2277,#2278));
#710=EDGE_LOOP('',(#2279,#2280,#2281,#2282));
#711=EDGE_LOOP('',(#2283,#2284,#2285,#2286));
#712=EDGE_LOOP('',(#2287));
#713=EDGE_LOOP('',(#2288));
#714=EDGE_LOOP('',(#2289));
#715=EDGE_LOOP('',(#2290));
#716=EDGE_LOOP('',(#2291));
#717=EDGE_LOOP('',(#2292,#2293,#2294,#2295));
#718=EDGE_LOOP('',(#2296));
#719=EDGE_LOOP('',(#2297));
#720=EDGE_LOOP('',(#2298));
#721=EDGE_LOOP('',(#2299));
#722=EDGE_LOOP('',(#2300));
#723=EDGE_LOOP('',(#2301,#2302,#2303,#2304));
#724=EDGE_LOOP('',(#2305,#2306,#2307,#2308));
#725=EDGE_LOOP('',(#2309,#2310,#2311,#2312));
#726=EDGE_LOOP('',(#2313,#2314,#2315,#2316));
#727=EDGE_LOOP('',(#2317,#2318,#2319,#2320));
#728=EDGE_LOOP('',(#2321,#2322,#2323,#2324));
#729=EDGE_LOOP('',(#2325,#2326,#2327,#2328));
#730=EDGE_LOOP('',(#2329,#2330,#2331,#2332));
#731=EDGE_LOOP('',(#2333,#2334,#2335,#2336));
#732=EDGE_LOOP('',(#2337));
#733=EDGE_LOOP('',(#2338));
#734=EDGE_LOOP('',(#2339));
#735=EDGE_LOOP('',(#2340));
#736=EDGE_LOOP('',(#2341));
#737=EDGE_LOOP('',(#2342,#2343,#2344,#2345));
#738=EDGE_LOOP('',(#2346));
#739=EDGE_LOOP('',(#2347));
#740=EDGE_LOOP('',(#2348));
#741=EDGE_LOOP('',(#2349));
#742=EDGE_LOOP('',(#2350));
#743=EDGE_LOOP('',(#2351,#2352,#2353,#2354));
#744=EDGE_LOOP('',(#2355,#2356,#2357,#2358));
#745=EDGE_LOOP('',(#2359,#2360,#2361,#2362));
#746=EDGE_LOOP('',(#2363,#2364,#2365,#2366));
#747=EDGE_LOOP('',(#2367,#2368,#2369,#2370));
#748=EDGE_LOOP('',(#2371,#2372,#2373,#2374));
#749=EDGE_LOOP('',(#2375,#2376,#2377,#2378));
#750=EDGE_LOOP('',(#2379,#2380,#2381,#2382));
#751=EDGE_LOOP('',(#2383,#2384,#2385,#2386));
#752=EDGE_LOOP('',(#2387,#2388,#2389,#2390));
#753=EDGE_LOOP('',(#2391));
#754=EDGE_LOOP('',(#2392));
#755=EDGE_LOOP('',(#2393));
#756=EDGE_LOOP('',(#2394));
#757=EDGE_LOOP('',(#2395,#2396,#2397,#2398));
#758=EDGE_LOOP('',(#2399,#2400,#2401,#2402));
#759=EDGE_LOOP('',(#2403));
#760=EDGE_LOOP('',(#2404));
#761=EDGE_LOOP('',(#2405));
#762=EDGE_LOOP('',(#2406));
#763=EDGE_LOOP('',(#2407,#2408,#2409,#2410));
#764=EDGE_LOOP('',(#2411,#2412,#2413,#2414));
#765=EDGE_LOOP('',(#2415));
#766=EDGE_LOOP('',(#2416));
#767=EDGE_LOOP('',(#2417));
#768=EDGE_LOOP('',(#2418));
#769=EDGE_LOOP('',(#2419,#2420,#2421,#2422));
#770=EDGE_LOOP('',(#2423,#2424,#2425,#2426));
#771=EDGE_LOOP('',(#2427));
#772=EDGE_LOOP('',(#2428));
#773=EDGE_LOOP('',(#2429));
#774=EDGE_LOOP('',(#2430));
#775=EDGE_LOOP('',(#2431,#2432,#2433,#2434));
#776=EDGE_LOOP('',(#2435,#2436,#2437,#2438));
#777=EDGE_LOOP('',(#2439));
#778=EDGE_LOOP('',(#2440));
#779=EDGE_LOOP('',(#2441));
#780=EDGE_LOOP('',(#2442));
#781=EDGE_LOOP('',(#2443,#2444,#2445,#2446));
#782=EDGE_LOOP('',(#2447,#2448,#2449,#2450));
#783=EDGE_LOOP('',(#2451));
#784=EDGE_LOOP('',(#2452));
#785=EDGE_LOOP('',(#2453));
#786=EDGE_LOOP('',(#2454));
#787=EDGE_LOOP('',(#2455,#2456,#2457,#2458));
#788=EDGE_LOOP('',(#2459,#2460,#2461,#2462));
#789=EDGE_LOOP('',(#2463));
#790=EDGE_LOOP('',(#2464));
#791=EDGE_LOOP('',(#2465));
#792=EDGE_LOOP('',(#2466));
#793=EDGE_LOOP('',(#2467,#2468,#2469,#2470));
#794=EDGE_LOOP('',(#2471,#2472,#2473,#2474));
#795=EDGE_LOOP('',(#2475));
#796=EDGE_LOOP('',(#2476));
#797=EDGE_LOOP('',(#2477));
#798=EDGE_LOOP('',(#2478));
#799=EDGE_LOOP('',(#2479,#2480,#2481,#2482));
#800=EDGE_LOOP('',(#2483,#2484,#2485,#2486));
#801=EDGE_LOOP('',(#2487,#2488));
#802=EDGE_LOOP('',(#2489));
#803=EDGE_LOOP('',(#2490));
#804=EDGE_LOOP('',(#2491,#2492,#2493,#2494));
#805=EDGE_LOOP('',(#2495,#2496,#2497,#2498));
#806=EDGE_LOOP('',(#2499));
#807=EDGE_LOOP('',(#2500));
#808=EDGE_LOOP('',(#2501));
#809=EDGE_LOOP('',(#2502));
#810=EDGE_LOOP('',(#2503,#2504,#2505,#2506));
#811=EDGE_LOOP('',(#2507,#2508,#2509,#2510));
#812=EDGE_LOOP('',(#2511,#2512,#2513,#2514));
#813=EDGE_LOOP('',(#2515,#2516,#2517,#2518));
#814=EDGE_LOOP('',(#2519,#2520,#2521,#2522));
#815=EDGE_LOOP('',(#2523,#2524,#2525,#2526));
#816=EDGE_LOOP('',(#2527,#2528,#2529,#2530));
#817=EDGE_LOOP('',(#2531,#2532,#2533,#2534));
#818=EDGE_LOOP('',(#2535,#2536,#2537,#2538));
#819=EDGE_LOOP('',(#2539,#2540,#2541,#2542));
#820=EDGE_LOOP('',(#2543,#2544,#2545,#2546));
#821=EDGE_LOOP('',(#2547,#2548,#2549,#2550));
#822=EDGE_LOOP('',(#2551,#2552,#2553,#2554,#2555,#2556,#2557,#2558));
#823=EDGE_LOOP('',(#2559));
#824=EDGE_LOOP('',(#2560));
#825=EDGE_LOOP('',(#2561));
#826=EDGE_LOOP('',(#2562));
#827=EDGE_LOOP('',(#2563));
#828=EDGE_LOOP('',(#2564,#2565,#2566,#2567,#2568,#2569,#2570,#2571));
#829=EDGE_LOOP('',(#2572));
#830=EDGE_LOOP('',(#2573));
#831=EDGE_LOOP('',(#2574));
#832=EDGE_LOOP('',(#2575));
#833=EDGE_LOOP('',(#2576));
#834=EDGE_LOOP('',(#2577,#2578,#2579,#2580));
#835=EDGE_LOOP('',(#2581));
#836=EDGE_LOOP('',(#2582));
#837=EDGE_LOOP('',(#2583,#2584));
#838=EDGE_LOOP('',(#2585));
#839=EDGE_LOOP('',(#2586));
#840=EDGE_LOOP('',(#2587));
#841=EDGE_LOOP('',(#2588));
#842=EDGE_LOOP('',(#2589,#2590,#2591,#2592,#2593,#2594));
#843=EDGE_LOOP('',(#2595,#2596,#2597,#2598,#2599,#2600));
#844=EDGE_LOOP('',(#2601,#2602,#2603,#2604));
#845=EDGE_LOOP('',(#2605,#2606,#2607));
#846=EDGE_LOOP('',(#2608,#2609,#2610));
#847=EDGE_LOOP('',(#2611,#2612,#2613));
#848=EDGE_LOOP('',(#2614,#2615,#2616));
#849=EDGE_LOOP('',(#2617,#2618,#2619));
#850=EDGE_LOOP('',(#2620,#2621,#2622));
#851=EDGE_LOOP('',(#2623,#2624,#2625,#2626,#2627,#2628));
#852=EDGE_LOOP('',(#2629,#2630,#2631,#2632,#2633,#2634));
#853=EDGE_LOOP('',(#2635,#2636,#2637,#2638,#2639,#2640));
#854=EDGE_LOOP('',(#2641,#2642,#2643,#2644,#2645,#2646));
#855=EDGE_LOOP('',(#2647));
#856=EDGE_LOOP('',(#2648));
#857=EDGE_LOOP('',(#2649));
#858=EDGE_LOOP('',(#2650));
#859=EDGE_LOOP('',(#2651,#2652,#2653,#2654));
#860=EDGE_LOOP('',(#2655));
#861=EDGE_LOOP('',(#2656));
#862=EDGE_LOOP('',(#2657,#2658,#2659,#2660));
#863=EDGE_LOOP('',(#2661));
#864=EDGE_LOOP('',(#2662));
#865=EDGE_LOOP('',(#2663));
#866=EDGE_LOOP('',(#2664));
#867=EDGE_LOOP('',(#2665));
#868=EDGE_LOOP('',(#2666));
#869=EDGE_LOOP('',(#2667,#2668,#2669,#2670));
#870=EDGE_LOOP('',(#2671,#2672,#2673,#2674));
#871=EDGE_LOOP('',(#2675));
#872=EDGE_LOOP('',(#2676));
#873=EDGE_LOOP('',(#2677));
#874=EDGE_LOOP('',(#2678));
#875=EDGE_LOOP('',(#2679));
#876=EDGE_LOOP('',(#2680,#2681,#2682,#2683));
#877=EDGE_LOOP('',(#2684,#2685,#2686,#2687));
#878=EDGE_LOOP('',(#2688,#2689,#2690,#2691));
#879=EDGE_LOOP('',(#2692));
#880=EDGE_LOOP('',(#2693));
#881=EDGE_LOOP('',(#2694,#2695,#2696,#2697));
#882=EDGE_LOOP('',(#2698,#2699,#2700,#2701));
#883=EDGE_LOOP('',(#2702,#2703,#2704,#2705));
#884=EDGE_LOOP('',(#2706));
#885=EDGE_LOOP('',(#2707,#2708,#2709,#2710));
#886=EDGE_LOOP('',(#2711,#2712,#2713,#2714));
#887=EDGE_LOOP('',(#2715,#2716,#2717,#2718));
#888=EDGE_LOOP('',(#2719,#2720,#2721,#2722));
#889=EDGE_LOOP('',(#2723,#2724,#2725,#2726));
#890=EDGE_LOOP('',(#2727,#2728,#2729,#2730));
#891=EDGE_LOOP('',(#2731,#2732,#2733,#2734,#2735,#2736));
#892=EDGE_LOOP('',(#2737,#2738,#2739,#2740,#2741,#2742));
#893=EDGE_LOOP('',(#2743,#2744,#2745,#2746));
#894=EDGE_LOOP('',(#2747,#2748,#2749,#2750));
#895=EDGE_LOOP('',(#2751,#2752,#2753,#2754));
#896=EDGE_LOOP('',(#2755,#2756,#2757,#2758));
#897=EDGE_LOOP('',(#2759,#2760,#2761,#2762));
#898=EDGE_LOOP('',(#2763,#2764,#2765,#2766));
#899=EDGE_LOOP('',(#2767,#2768,#2769,#2770));
#900=EDGE_LOOP('',(#2771));
#901=EDGE_LOOP('',(#2772));
#902=EDGE_LOOP('',(#2773));
#903=EDGE_LOOP('',(#2774,#2775,#2776,#2777));
#904=EDGE_LOOP('',(#2778,#2779,#2780,#2781));
#905=EDGE_LOOP('',(#2782));
#906=EDGE_LOOP('',(#2783));
#907=EDGE_LOOP('',(#2784,#2785,#2786,#2787));
#908=EDGE_LOOP('',(#2788));
#909=EDGE_LOOP('',(#2789,#2790,#2791,#2792,#2793,#2794));
#910=EDGE_LOOP('',(#2795,#2796,#2797,#2798,#2799,#2800,#2801,#2802));
#911=EDGE_LOOP('',(#2803,#2804,#2805,#2806));
#912=EDGE_LOOP('',(#2807,#2808,#2809,#2810));
#913=EDGE_LOOP('',(#2811,#2812,#2813,#2814));
#914=EDGE_LOOP('',(#2815));
#915=EDGE_LOOP('',(#2816,#2817,#2818,#2819));
#916=EDGE_LOOP('',(#2820,#2821,#2822,#2823));
#917=EDGE_LOOP('',(#2824,#2825));
#918=EDGE_LOOP('',(#2826,#2827,#2828,#2829,#2830,#2831));
#919=EDGE_LOOP('',(#2832,#2833,#2834,#2835,#2836,#2837));
#920=EDGE_LOOP('',(#2838,#2839,#2840,#2841,#2842,#2843));
#921=EDGE_LOOP('',(#2844));
#922=EDGE_LOOP('',(#2845,#2846,#2847,#2848));
#923=EDGE_LOOP('',(#2849,#2850,#2851,#2852,#2853,#2854,#2855,#2856,#2857,
#2858));
#924=EDGE_LOOP('',(#2859));
#925=EDGE_LOOP('',(#2860));
#926=EDGE_LOOP('',(#2861));
#927=EDGE_LOOP('',(#2862,#2863,#2864,#2865,#2866,#2867,#2868,#2869,#2870,
#2871,#2872,#2873,#2874,#2875,#2876,#2877,#2878,#2879,#2880));
#928=EDGE_LOOP('',(#2881,#2882));
#929=EDGE_LOOP('',(#2883,#2884));
#930=EDGE_LOOP('',(#2885,#2886,#2887,#2888));
#931=EDGE_LOOP('',(#2889,#2890,#2891,#2892));
#932=EDGE_LOOP('',(#2893,#2894,#2895,#2896));
#933=EDGE_LOOP('',(#2897,#2898,#2899,#2900));
#934=EDGE_LOOP('',(#2901,#2902,#2903,#2904));
#935=EDGE_LOOP('',(#2905,#2906,#2907,#2908));
#936=EDGE_LOOP('',(#2909,#2910,#2911,#2912));
#937=EDGE_LOOP('',(#2913,#2914,#2915,#2916));
#938=EDGE_LOOP('',(#2917,#2918,#2919,#2920));
#939=EDGE_LOOP('',(#2921,#2922,#2923,#2924));
#940=EDGE_LOOP('',(#2925,#2926,#2927,#2928));
#941=EDGE_LOOP('',(#2929,#2930,#2931,#2932));
#942=EDGE_LOOP('',(#2933,#2934,#2935,#2936));
#943=EDGE_LOOP('',(#2937,#2938,#2939,#2940));
#944=EDGE_LOOP('',(#2941,#2942,#2943,#2944));
#945=EDGE_LOOP('',(#2945,#2946,#2947,#2948));
#946=EDGE_LOOP('',(#2949,#2950,#2951,#2952));
#947=EDGE_LOOP('',(#2953,#2954,#2955,#2956));
#948=EDGE_LOOP('',(#2957,#2958,#2959,#2960));
#949=EDGE_LOOP('',(#2961,#2962,#2963,#2964));
#950=EDGE_LOOP('',(#2965,#2966,#2967,#2968,#2969,#2970));
#951=EDGE_LOOP('',(#2971));
#952=EDGE_LOOP('',(#2972,#2973,#2974,#2975,#2976,#2977));
#953=EDGE_LOOP('',(#2978,#2979,#2980,#2981));
#954=EDGE_LOOP('',(#2982,#2983,#2984,#2985));
#955=EDGE_LOOP('',(#2986,#2987,#2988,#2989));
#956=EDGE_LOOP('',(#2990));
#957=EDGE_LOOP('',(#2991,#2992,#2993,#2994));
#958=EDGE_LOOP('',(#2995));
#959=EDGE_LOOP('',(#2996));
#960=EDGE_LOOP('',(#2997,#2998,#2999,#3000));
#961=EDGE_LOOP('',(#3001,#3002,#3003,#3004));
#962=EDGE_LOOP('',(#3005));
#963=EDGE_LOOP('',(#3006,#3007,#3008,#3009));
#964=EDGE_LOOP('',(#3010));
#965=EDGE_LOOP('',(#3011));
#966=EDGE_LOOP('',(#3012,#3013,#3014,#3015));
#967=EDGE_LOOP('',(#3016));
#968=EDGE_LOOP('',(#3017,#3018,#3019,#3020));
#969=EDGE_LOOP('',(#3021,#3022,#3023,#3024));
#970=EDGE_LOOP('',(#3025,#3026,#3027,#3028));
#971=EDGE_LOOP('',(#3029,#3030,#3031,#3032));
#972=EDGE_LOOP('',(#3033,#3034,#3035,#3036));
#973=EDGE_LOOP('',(#3037,#3038,#3039,#3040));
#974=EDGE_LOOP('',(#3041,#3042,#3043,#3044,#3045,#3046));
#975=EDGE_LOOP('',(#3047));
#976=EDGE_LOOP('',(#3048,#3049,#3050,#3051,#3052,#3053));
#977=EDGE_LOOP('',(#3054,#3055,#3056,#3057));
#978=EDGE_LOOP('',(#3058,#3059,#3060,#3061));
#979=EDGE_LOOP('',(#3062,#3063,#3064,#3065));
#980=EDGE_LOOP('',(#3066));
#981=LINE('',#4939,#1209);
#982=LINE('',#4945,#1210);
#983=LINE('',#4951,#1211);
#984=LINE('',#4957,#1212);
#985=LINE('',#4963,#1213);
#986=LINE('',#4968,#1214);
#987=LINE('',#4970,#1215);
#988=LINE('',#4972,#1216);
#989=LINE('',#4973,#1217);
#990=LINE('',#4977,#1218);
#991=LINE('',#4979,#1219);
#992=LINE('',#4981,#1220);
#993=LINE('',#4982,#1221);
#994=LINE('',#4984,#1222);
#995=LINE('',#4985,#1223);
#996=LINE('',#4987,#1224);
#997=LINE('',#4989,#1225);
#998=LINE('',#4994,#1226);
#999=LINE('',#5000,#1227);
#1000=LINE('',#5006,#1228);
#1001=LINE('',#5012,#1229);
#1002=LINE('',#5018,#1230);
#1003=LINE('',#5023,#1231);
#1004=LINE('',#5025,#1232);
#1005=LINE('',#5027,#1233);
#1006=LINE('',#5028,#1234);
#1007=LINE('',#5032,#1235);
#1008=LINE('',#5034,#1236);
#1009=LINE('',#5036,#1237);
#1010=LINE('',#5037,#1238);
#1011=LINE('',#5039,#1239);
#1012=LINE('',#5040,#1240);
#1013=LINE('',#5042,#1241);
#1014=LINE('',#5044,#1242);
#1015=LINE('',#5048,#1243);
#1016=LINE('',#5050,#1244);
#1017=LINE('',#5052,#1245);
#1018=LINE('',#5053,#1246);
#1019=LINE('',#5056,#1247);
#1020=LINE('',#5058,#1248);
#1021=LINE('',#5059,#1249);
#1022=LINE('',#5062,#1250);
#1023=LINE('',#5064,#1251);
#1024=LINE('',#5065,#1252);
#1025=LINE('',#5067,#1253);
#1026=LINE('',#5068,#1254);
#1027=LINE('',#5076,#1255);
#1028=LINE('',#5082,#1256);
#1029=LINE('',#5091,#1257);
#1030=LINE('',#5097,#1258);
#1031=LINE('',#5106,#1259);
#1032=LINE('',#5112,#1260);
#1033=LINE('',#5121,#1261);
#1034=LINE('',#5127,#1262);
#1035=LINE('',#5136,#1263);
#1036=LINE('',#5142,#1264);
#1037=LINE('',#5151,#1265);
#1038=LINE('',#5157,#1266);
#1039=LINE('',#5166,#1267);
#1040=LINE('',#5172,#1268);
#1041=LINE('',#5181,#1269);
#1042=LINE('',#5187,#1270);
#1043=LINE('',#5197,#1271);
#1044=LINE('',#5203,#1272);
#1045=LINE('',#5213,#1273);
#1046=LINE('',#5219,#1274);
#1047=LINE('',#5227,#1275);
#1048=LINE('',#5233,#1276);
#1049=LINE('',#5239,#1277);
#1050=LINE('',#5245,#1278);
#1051=LINE('',#5250,#1279);
#1052=LINE('',#5252,#1280);
#1053=LINE('',#5254,#1281);
#1054=LINE('',#5255,#1282);
#1055=LINE('',#5258,#1283);
#1056=LINE('',#5260,#1284);
#1057=LINE('',#5261,#1285);
#1058=LINE('',#5264,#1286);
#1059=LINE('',#5266,#1287);
#1060=LINE('',#5267,#1288);
#1061=LINE('',#5270,#1289);
#1062=LINE('',#5272,#1290);
#1063=LINE('',#5273,#1291);
#1064=LINE('',#5276,#1292);
#1065=LINE('',#5278,#1293);
#1066=LINE('',#5279,#1294);
#1067=LINE('',#5282,#1295);
#1068=LINE('',#5284,#1296);
#1069=LINE('',#5285,#1297);
#1070=LINE('',#5288,#1298);
#1071=LINE('',#5290,#1299);
#1072=LINE('',#5291,#1300);
#1073=LINE('',#5293,#1301);
#1074=LINE('',#5294,#1302);
#1075=LINE('',#5302,#1303);
#1076=LINE('',#5357,#1304);
#1077=LINE('',#5429,#1305);
#1078=LINE('',#5474,#1306);
#1079=LINE('',#5642,#1307);
#1080=LINE('',#5713,#1308);
#1081=LINE('',#5716,#1309);
#1082=LINE('',#5787,#1310);
#1083=LINE('',#5797,#1311);
#1084=LINE('',#5802,#1312);
#1085=LINE('',#5810,#1313);
#1086=LINE('',#5816,#1314);
#1087=LINE('',#5827,#1315);
#1088=LINE('',#5831,#1316);
#1089=LINE('',#5835,#1317);
#1090=LINE('',#5842,#1318);
#1091=LINE('',#5846,#1319);
#1092=LINE('',#5850,#1320);
#1093=LINE('',#5855,#1321);
#1094=LINE('',#5857,#1322);
#1095=LINE('',#5859,#1323);
#1096=LINE('',#5860,#1324);
#1097=LINE('',#5863,#1325);
#1098=LINE('',#5865,#1326);
#1099=LINE('',#5866,#1327);
#1100=LINE('',#5869,#1328);
#1101=LINE('',#5871,#1329);
#1102=LINE('',#5872,#1330);
#1103=LINE('',#5875,#1331);
#1104=LINE('',#5877,#1332);
#1105=LINE('',#5878,#1333);
#1106=LINE('',#5881,#1334);
#1107=LINE('',#5883,#1335);
#1108=LINE('',#5884,#1336);
#1109=LINE('',#5886,#1337);
#1110=LINE('',#5887,#1338);
#1111=LINE('',#5922,#1339);
#1112=LINE('',#5924,#1340);
#1113=LINE('',#5926,#1341);
#1114=LINE('',#5927,#1342);
#1115=LINE('',#5932,#1343);
#1116=LINE('',#5933,#1344);
#1117=LINE('',#5936,#1345);
#1118=LINE('',#5937,#1346);
#1119=LINE('',#5940,#1347);
#1120=LINE('',#5941,#1348);
#1121=LINE('',#5948,#1349);
#1122=LINE('',#5960,#1350);
#1123=LINE('',#5964,#1351);
#1124=LINE('',#5971,#1352);
#1125=LINE('',#6033,#1353);
#1126=LINE('',#6131,#1354);
#1127=LINE('',#6178,#1355);
#1128=LINE('',#6180,#1356);
#1129=LINE('',#6182,#1357);
#1130=LINE('',#6183,#1358);
#1131=LINE('',#6187,#1359);
#1132=LINE('',#6189,#1360);
#1133=LINE('',#6191,#1361);
#1134=LINE('',#6192,#1362);
#1135=LINE('',#6194,#1363);
#1136=LINE('',#6195,#1364);
#1137=LINE('',#6233,#1365);
#1138=LINE('',#6323,#1366);
#1139=LINE('',#6411,#1367);
#1140=LINE('',#6474,#1368);
#1141=LINE('',#6475,#1369);
#1142=LINE('',#6488,#1370);
#1143=LINE('',#6490,#1371);
#1144=LINE('',#6492,#1372);
#1145=LINE('',#6493,#1373);
#1146=LINE('',#6497,#1374);
#1147=LINE('',#6503,#1375);
#1148=LINE('',#6504,#1376);
#1149=LINE('',#6505,#1377);
#1150=LINE('',#6511,#1378);
#1151=LINE('',#6514,#1379);
#1152=LINE('',#6517,#1380);
#1153=LINE('',#6518,#1381);
#1154=LINE('',#6522,#1382);
#1155=LINE('',#6524,#1383);
#1156=LINE('',#6525,#1384);
#1157=LINE('',#6528,#1385);
#1158=LINE('',#6533,#1386);
#1159=LINE('',#6534,#1387);
#1160=LINE('',#6535,#1388);
#1161=LINE('',#6540,#1389);
#1162=LINE('',#6547,#1390);
#1163=LINE('',#6549,#1391);
#1164=LINE('',#6551,#1392);
#1165=LINE('',#6552,#1393);
#1166=LINE('',#6555,#1394);
#1167=LINE('',#6557,#1395);
#1168=LINE('',#6558,#1396);
#1169=LINE('',#6561,#1397);
#1170=LINE('',#6563,#1398);
#1171=LINE('',#6564,#1399);
#1172=LINE('',#6567,#1400);
#1173=LINE('',#6569,#1401);
#1174=LINE('',#6570,#1402);
#1175=LINE('',#6573,#1403);
#1176=LINE('',#6575,#1404);
#1177=LINE('',#6576,#1405);
#1178=LINE('',#6578,#1406);
#1179=LINE('',#6579,#1407);
#1180=LINE('',#6587,#1408);
#1181=LINE('',#6591,#1409);
#1182=LINE('',#6595,#1410);
#1183=LINE('',#6635,#1411);
#1184=LINE('',#6678,#1412);
#1185=LINE('',#6682,#1413);
#1186=LINE('',#6686,#1414);
#1187=LINE('',#6691,#1415);
#1188=LINE('',#6696,#1416);
#1189=LINE('',#6698,#1417);
#1190=LINE('',#6700,#1418);
#1191=LINE('',#6701,#1419);
#1192=LINE('',#6704,#1420);
#1193=LINE('',#6706,#1421);
#1194=LINE('',#6707,#1422);
#1195=LINE('',#6710,#1423);
#1196=LINE('',#6712,#1424);
#1197=LINE('',#6713,#1425);
#1198=LINE('',#6716,#1426);
#1199=LINE('',#6718,#1427);
#1200=LINE('',#6719,#1428);
#1201=LINE('',#6722,#1429);
#1202=LINE('',#6724,#1430);
#1203=LINE('',#6725,#1431);
#1204=LINE('',#6727,#1432);
#1205=LINE('',#6728,#1433);
#1206=LINE('',#6736,#1434);
#1207=LINE('',#6740,#1435);
#1208=LINE('',#6744,#1436);
#1209=VECTOR('',#3946,0.34);
#1210=VECTOR('',#3953,0.34);
#1211=VECTOR('',#3960,0.34);
#1212=VECTOR('',#3967,0.34);
#1213=VECTOR('',#3974,3.01);
#1214=VECTOR('',#3979,1.);
#1215=VECTOR('',#3980,1.);
#1216=VECTOR('',#3981,1.);
#1217=VECTOR('',#3982,1.);
#1218=VECTOR('',#3985,1.);
#1219=VECTOR('',#3986,1.);
#1220=VECTOR('',#3987,1.);
#1221=VECTOR('',#3988,1.);
#1222=VECTOR('',#3991,1.);
#1223=VECTOR('',#3992,1.);
#1224=VECTOR('',#3995,1.);
#1225=VECTOR('',#3998,1.);
#1226=VECTOR('',#4003,0.34);
#1227=VECTOR('',#4010,0.34);
#1228=VECTOR('',#4017,0.34);
#1229=VECTOR('',#4024,0.34);
#1230=VECTOR('',#4031,3.01);
#1231=VECTOR('',#4036,1.);
#1232=VECTOR('',#4037,1.);
#1233=VECTOR('',#4038,1.);
#1234=VECTOR('',#4039,1.);
#1235=VECTOR('',#4042,1.);
#1236=VECTOR('',#4043,1.);
#1237=VECTOR('',#4044,1.);
#1238=VECTOR('',#4045,1.);
#1239=VECTOR('',#4048,1.);
#1240=VECTOR('',#4049,1.);
#1241=VECTOR('',#4052,1.);
#1242=VECTOR('',#4055,1.);
#1243=VECTOR('',#4058,1.);
#1244=VECTOR('',#4059,1.);
#1245=VECTOR('',#4060,1.);
#1246=VECTOR('',#4061,1.);
#1247=VECTOR('',#4064,1.);
#1248=VECTOR('',#4065,1.);
#1249=VECTOR('',#4066,1.);
#1250=VECTOR('',#4069,1.);
#1251=VECTOR('',#4070,1.);
#1252=VECTOR('',#4071,1.);
#1253=VECTOR('',#4074,1.);
#1254=VECTOR('',#4075,1.);
#1255=VECTOR('',#4086,0.425);
#1256=VECTOR('',#4093,0.595);
#1257=VECTOR('',#4106,0.425);
#1258=VECTOR('',#4113,0.595);
#1259=VECTOR('',#4126,0.425);
#1260=VECTOR('',#4133,0.595);
#1261=VECTOR('',#4146,0.425);
#1262=VECTOR('',#4153,0.595);
#1263=VECTOR('',#4166,0.425);
#1264=VECTOR('',#4173,0.595);
#1265=VECTOR('',#4186,0.425);
#1266=VECTOR('',#4193,0.595);
#1267=VECTOR('',#4206,0.425);
#1268=VECTOR('',#4213,0.595);
#1269=VECTOR('',#4226,0.425);
#1270=VECTOR('',#4233,0.595);
#1271=VECTOR('',#4248,2.05);
#1272=VECTOR('',#4255,2.05);
#1273=VECTOR('',#4266,3.);
#1274=VECTOR('',#4273,3.);
#1275=VECTOR('',#4284,0.6);
#1276=VECTOR('',#4291,0.6);
#1277=VECTOR('',#4298,0.6);
#1278=VECTOR('',#4305,0.6);
#1279=VECTOR('',#4310,1.);
#1280=VECTOR('',#4311,1.);
#1281=VECTOR('',#4312,1.);
#1282=VECTOR('',#4313,1.);
#1283=VECTOR('',#4316,1.);
#1284=VECTOR('',#4317,1.);
#1285=VECTOR('',#4318,1.);
#1286=VECTOR('',#4321,1.);
#1287=VECTOR('',#4322,1.);
#1288=VECTOR('',#4323,1.);
#1289=VECTOR('',#4326,1.);
#1290=VECTOR('',#4327,1.);
#1291=VECTOR('',#4328,1.);
#1292=VECTOR('',#4331,1.);
#1293=VECTOR('',#4332,1.);
#1294=VECTOR('',#4333,1.);
#1295=VECTOR('',#4336,1.);
#1296=VECTOR('',#4337,1.);
#1297=VECTOR('',#4338,1.);
#1298=VECTOR('',#4341,1.);
#1299=VECTOR('',#4342,1.);
#1300=VECTOR('',#4343,1.);
#1301=VECTOR('',#4346,1.);
#1302=VECTOR('',#4347,1.);
#1303=VECTOR('',#4358,1.8);
#1304=VECTOR('',#4375,0.25);
#1305=VECTOR('',#4378,0.25);
#1306=VECTOR('',#4383,1.65);
#1307=VECTOR('',#4388,0.25);
#1308=VECTOR('',#4391,0.25);
#1309=VECTOR('',#4394,0.25);
#1310=VECTOR('',#4397,0.25);
#1311=VECTOR('',#4410,1.75);
#1312=VECTOR('',#4417,0.6);
#1313=VECTOR('',#4428,0.42);
#1314=VECTOR('',#4435,0.8);
#1315=VECTOR('',#4452,0.625);
#1316=VECTOR('',#4457,0.65);
#1317=VECTOR('',#4462,0.635);
#1318=VECTOR('',#4471,0.41);
#1319=VECTOR('',#4476,0.4);
#1320=VECTOR('',#4481,0.36);
#1321=VECTOR('',#4486,1.);
#1322=VECTOR('',#4487,1.);
#1323=VECTOR('',#4488,1.);
#1324=VECTOR('',#4489,1.);
#1325=VECTOR('',#4492,1.);
#1326=VECTOR('',#4493,1.);
#1327=VECTOR('',#4494,1.);
#1328=VECTOR('',#4497,1.);
#1329=VECTOR('',#4498,1.);
#1330=VECTOR('',#4499,1.);
#1331=VECTOR('',#4502,1.);
#1332=VECTOR('',#4503,1.);
#1333=VECTOR('',#4504,1.);
#1334=VECTOR('',#4507,1.);
#1335=VECTOR('',#4508,1.);
#1336=VECTOR('',#4509,1.);
#1337=VECTOR('',#4512,1.);
#1338=VECTOR('',#4513,1.);
#1339=VECTOR('',#4578,1.);
#1340=VECTOR('',#4579,1.);
#1341=VECTOR('',#4580,1.);
#1342=VECTOR('',#4581,1.);
#1343=VECTOR('',#4586,1.);
#1344=VECTOR('',#4587,1.);
#1345=VECTOR('',#4590,1.);
#1346=VECTOR('',#4591,1.);
#1347=VECTOR('',#4594,1.);
#1348=VECTOR('',#4595,1.);
#1349=VECTOR('',#4604,0.6);
#1350=VECTOR('',#4623,0.699999999999999);
#1351=VECTOR('',#4628,0.8);
#1352=VECTOR('',#4637,0.399999999999999);
#1353=VECTOR('',#4642,0.4);
#1354=VECTOR('',#4645,0.25);
#1355=VECTOR('',#4648,1.);
#1356=VECTOR('',#4649,1.);
#1357=VECTOR('',#4650,1.);
#1358=VECTOR('',#4651,1.);
#1359=VECTOR('',#4654,1.);
#1360=VECTOR('',#4655,1.);
#1361=VECTOR('',#4656,1.);
#1362=VECTOR('',#4657,1.);
#1363=VECTOR('',#4660,1.);
#1364=VECTOR('',#4661,1.);
#1365=VECTOR('',#4674,0.4);
#1366=VECTOR('',#4677,0.4);
#1367=VECTOR('',#4680,0.4);
#1368=VECTOR('',#4687,1.6);
#1369=VECTOR('',#4688,1.6);
#1370=VECTOR('',#4707,1.);
#1371=VECTOR('',#4708,1.);
#1372=VECTOR('',#4709,1.);
#1373=VECTOR('',#4710,1.);
#1374=VECTOR('',#4713,1.);
#1375=VECTOR('',#4720,1.);
#1376=VECTOR('',#4721,1.);
#1377=VECTOR('',#4722,1.);
#1378=VECTOR('',#4731,1.);
#1379=VECTOR('',#4734,1.);
#1380=VECTOR('',#4737,1.);
#1381=VECTOR('',#4738,1.);
#1382=VECTOR('',#4743,1.);
#1383=VECTOR('',#4744,1.);
#1384=VECTOR('',#4745,1.);
#1385=VECTOR('',#4748,1.);
#1386=VECTOR('',#4753,1.);
#1387=VECTOR('',#4754,1.);
#1388=VECTOR('',#4755,1.);
#1389=VECTOR('',#4764,1.);
#1390=VECTOR('',#4773,1.);
#1391=VECTOR('',#4774,1.);
#1392=VECTOR('',#4775,1.);
#1393=VECTOR('',#4776,1.);
#1394=VECTOR('',#4779,1.);
#1395=VECTOR('',#4780,1.);
#1396=VECTOR('',#4781,1.);
#1397=VECTOR('',#4784,1.);
#1398=VECTOR('',#4785,1.);
#1399=VECTOR('',#4786,1.);
#1400=VECTOR('',#4789,1.);
#1401=VECTOR('',#4790,1.);
#1402=VECTOR('',#4791,1.);
#1403=VECTOR('',#4794,1.);
#1404=VECTOR('',#4795,1.);
#1405=VECTOR('',#4796,1.);
#1406=VECTOR('',#4799,1.);
#1407=VECTOR('',#4800,1.);
#1408=VECTOR('',#4811,0.285);
#1409=VECTOR('',#4816,0.3);
#1410=VECTOR('',#4821,0.25);
#1411=VECTOR('',#4828,0.21);
#1412=VECTOR('',#4839,1.075);
#1413=VECTOR('',#4844,1.1);
#1414=VECTOR('',#4849,1.075);
#1415=VECTOR('',#4856,0.6);
#1416=VECTOR('',#4861,1.);
#1417=VECTOR('',#4862,1.);
#1418=VECTOR('',#4863,1.);
#1419=VECTOR('',#4864,1.);
#1420=VECTOR('',#4867,1.);
#1421=VECTOR('',#4868,1.);
#1422=VECTOR('',#4869,1.);
#1423=VECTOR('',#4872,1.);
#1424=VECTOR('',#4873,1.);
#1425=VECTOR('',#4874,1.);
#1426=VECTOR('',#4877,1.);
#1427=VECTOR('',#4878,1.);
#1428=VECTOR('',#4879,1.);
#1429=VECTOR('',#4882,1.);
#1430=VECTOR('',#4883,1.);
#1431=VECTOR('',#4884,1.);
#1432=VECTOR('',#4887,1.);
#1433=VECTOR('',#4888,1.);
#1434=VECTOR('',#4899,0.235);
#1435=VECTOR('',#4904,0.25);
#1436=VECTOR('',#4909,0.2125);
#1437=CIRCLE('',#3556,0.34);
#1438=CIRCLE('',#3557,0.34);
#1439=CIRCLE('',#3559,0.34);
#1440=CIRCLE('',#3560,0.34);
#1441=CIRCLE('',#3562,0.34);
#1442=CIRCLE('',#3563,0.34);
#1443=CIRCLE('',#3565,0.34);
#1444=CIRCLE('',#3566,0.34);
#1445=CIRCLE('',#3568,3.01);
#1446=CIRCLE('',#3569,3.01);
#1447=CIRCLE('',#3576,0.34);
#1448=CIRCLE('',#3577,0.34);
#1449=CIRCLE('',#3579,0.34);
#1450=CIRCLE('',#3580,0.34);
#1451=CIRCLE('',#3582,0.34);
#1452=CIRCLE('',#3583,0.34);
#1453=CIRCLE('',#3585,0.34);
#1454=CIRCLE('',#3586,0.34);
#1455=CIRCLE('',#3588,3.01);
#1456=CIRCLE('',#3589,3.01);
#1457=CIRCLE('',#3603,0.425);
#1458=CIRCLE('',#3604,0.425);
#1459=CIRCLE('',#3606,0.595);
#1460=CIRCLE('',#3607,0.595);
#1461=CIRCLE('',#3612,0.425);
#1462=CIRCLE('',#3613,0.425);
#1463=CIRCLE('',#3615,0.595);
#1464=CIRCLE('',#3616,0.595);
#1465=CIRCLE('',#3621,0.425);
#1466=CIRCLE('',#3622,0.425);
#1467=CIRCLE('',#3624,0.595);
#1468=CIRCLE('',#3625,0.595);
#1469=CIRCLE('',#3630,0.425);
#1470=CIRCLE('',#3631,0.425);
#1471=CIRCLE('',#3633,0.595);
#1472=CIRCLE('',#3634,0.595);
#1473=CIRCLE('',#3639,0.425);
#1474=CIRCLE('',#3640,0.425);
#1475=CIRCLE('',#3642,0.595);
#1476=CIRCLE('',#3643,0.595);
#1477=CIRCLE('',#3648,0.425);
#1478=CIRCLE('',#3649,0.425);
#1479=CIRCLE('',#3651,0.595);
#1480=CIRCLE('',#3652,0.595);
#1481=CIRCLE('',#3657,0.425);
#1482=CIRCLE('',#3658,0.425);
#1483=CIRCLE('',#3660,0.595);
#1484=CIRCLE('',#3661,0.595);
#1485=CIRCLE('',#3666,0.425);
#1486=CIRCLE('',#3667,0.425);
#1487=CIRCLE('',#3669,0.595);
#1488=CIRCLE('',#3670,0.595);
#1489=CIRCLE('',#3676,2.05);
#1490=CIRCLE('',#3677,2.05);
#1491=CIRCLE('',#3679,2.05);
#1492=CIRCLE('',#3680,2.05);
#1493=CIRCLE('',#3682,2.35);
#1494=CIRCLE('',#3684,3.);
#1495=CIRCLE('',#3685,3.);
#1496=CIRCLE('',#3687,3.);
#1497=CIRCLE('',#3688,3.);
#1498=CIRCLE('',#3692,0.6);
#1499=CIRCLE('',#3693,0.6);
#1500=CIRCLE('',#3695,0.6);
#1501=CIRCLE('',#3696,0.6);
#1502=CIRCLE('',#3698,0.6);
#1503=CIRCLE('',#3699,0.6);
#1504=CIRCLE('',#3701,0.6);
#1505=CIRCLE('',#3702,0.6);
#1506=CIRCLE('',#3715,1.8);
#1507=CIRCLE('',#3716,1.8);
#1508=CIRCLE('',#3718,2.19089023002066);
#1509=CIRCLE('',#3720,2.35);
#1510=CIRCLE('',#3721,2.19089023002066);
#1511=CIRCLE('',#3726,1.65);
#1512=CIRCLE('',#3727,1.65);
#1513=CIRCLE('',#3733,0.6);
#1514=CIRCLE('',#3735,1.75);
#1515=CIRCLE('',#3737,1.75);
#1516=CIRCLE('',#3739,0.6);
#1517=CIRCLE('',#3745,0.42);
#1518=CIRCLE('',#3746,0.42);
#1519=CIRCLE('',#3748,0.8);
#1520=CIRCLE('',#3749,0.8);
#1521=CIRCLE('',#3754,0.6);
#1522=CIRCLE('',#3756,0.65);
#1523=CIRCLE('',#3758,0.65);
#1524=CIRCLE('',#3760,0.62);
#1525=CIRCLE('',#3762,0.42);
#1526=CIRCLE('',#3764,0.3933);
#1527=CIRCLE('',#3766,0.3933);
#1528=CIRCLE('',#3768,0.32);
#1529=CIRCLE('',#3809,0.6);
#1530=CIRCLE('',#3813,0.6);
#1531=CIRCLE('',#3815,0.6);
#1532=CIRCLE('',#3816,0.6);
#1533=CIRCLE('',#3822,0.6);
#1534=CIRCLE('',#3824,0.8);
#1535=CIRCLE('',#3826,0.8);
#1536=CIRCLE('',#3828,0.399999999999999);
#1537=CIRCLE('',#3830,0.399999999999999);
#1538=CIRCLE('',#3838,1.6);
#1539=CIRCLE('',#3839,0.6);
#1540=CIRCLE('',#3841,0.6);
#1541=CIRCLE('',#3846,1.6);
#1542=CIRCLE('',#3849,0.6);
#1543=CIRCLE('',#3850,3.8);
#1544=CIRCLE('',#3851,3.8);
#1545=CIRCLE('',#3852,3.8);
#1546=CIRCLE('',#3853,3.8);
#1547=CIRCLE('',#3858,0.16);
#1548=CIRCLE('',#3859,0.2);
#1549=CIRCLE('',#3862,0.16);
#1550=CIRCLE('',#3863,0.2);
#1551=CIRCLE('',#3865,0.2);
#1552=CIRCLE('',#3870,0.16);
#1553=CIRCLE('',#3873,0.2);
#1554=CIRCLE('',#3874,0.16);
#1555=CIRCLE('',#3887,0.27);
#1556=CIRCLE('',#3889,0.2942);
#1557=CIRCLE('',#3891,0.2942);
#1558=CIRCLE('',#3893,0.2);
#1559=CIRCLE('',#3898,1.05);
#1560=CIRCLE('',#3899,0.6);
#1561=CIRCLE('',#3901,1.1);
#1562=CIRCLE('',#3903,1.1);
#1563=CIRCLE('',#3905,1.05);
#1564=CIRCLE('',#3907,0.6);
#1565=CIRCLE('',#3918,0.22);
#1566=CIRCLE('',#3920,0.24505);
#1567=CIRCLE('',#3922,0.24505);
#1568=CIRCLE('',#3924,0.175);
#1569=VERTEX_POINT('',#4936);
#1570=VERTEX_POINT('',#4938);
#1571=VERTEX_POINT('',#4942);
#1572=VERTEX_POINT('',#4944);
#1573=VERTEX_POINT('',#4948);
#1574=VERTEX_POINT('',#4950);
#1575=VERTEX_POINT('',#4954);
#1576=VERTEX_POINT('',#4956);
#1577=VERTEX_POINT('',#4960);
#1578=VERTEX_POINT('',#4962);
#1579=VERTEX_POINT('',#4966);
#1580=VERTEX_POINT('',#4967);
#1581=VERTEX_POINT('',#4969);
#1582=VERTEX_POINT('',#4971);
#1583=VERTEX_POINT('',#4975);
#1584=VERTEX_POINT('',#4976);
#1585=VERTEX_POINT('',#4978);
#1586=VERTEX_POINT('',#4980);
#1587=VERTEX_POINT('',#4991);
#1588=VERTEX_POINT('',#4993);
#1589=VERTEX_POINT('',#4997);
#1590=VERTEX_POINT('',#4999);
#1591=VERTEX_POINT('',#5003);
#1592=VERTEX_POINT('',#5005);
#1593=VERTEX_POINT('',#5009);
#1594=VERTEX_POINT('',#5011);
#1595=VERTEX_POINT('',#5015);
#1596=VERTEX_POINT('',#5017);
#1597=VERTEX_POINT('',#5021);
#1598=VERTEX_POINT('',#5022);
#1599=VERTEX_POINT('',#5024);
#1600=VERTEX_POINT('',#5026);
#1601=VERTEX_POINT('',#5030);
#1602=VERTEX_POINT('',#5031);
#1603=VERTEX_POINT('',#5033);
#1604=VERTEX_POINT('',#5035);
#1605=VERTEX_POINT('',#5046);
#1606=VERTEX_POINT('',#5047);
#1607=VERTEX_POINT('',#5049);
#1608=VERTEX_POINT('',#5051);
#1609=VERTEX_POINT('',#5055);
#1610=VERTEX_POINT('',#5057);
#1611=VERTEX_POINT('',#5061);
#1612=VERTEX_POINT('',#5063);
#1613=VERTEX_POINT('',#5073);
#1614=VERTEX_POINT('',#5075);
#1615=VERTEX_POINT('',#5079);
#1616=VERTEX_POINT('',#5081);
#1617=VERTEX_POINT('',#5088);
#1618=VERTEX_POINT('',#5090);
#1619=VERTEX_POINT('',#5094);
#1620=VERTEX_POINT('',#5096);
#1621=VERTEX_POINT('',#5103);
#1622=VERTEX_POINT('',#5105);
#1623=VERTEX_POINT('',#5109);
#1624=VERTEX_POINT('',#5111);
#1625=VERTEX_POINT('',#5118);
#1626=VERTEX_POINT('',#5120);
#1627=VERTEX_POINT('',#5124);
#1628=VERTEX_POINT('',#5126);
#1629=VERTEX_POINT('',#5133);
#1630=VERTEX_POINT('',#5135);
#1631=VERTEX_POINT('',#5139);
#1632=VERTEX_POINT('',#5141);
#1633=VERTEX_POINT('',#5148);
#1634=VERTEX_POINT('',#5150);
#1635=VERTEX_POINT('',#5154);
#1636=VERTEX_POINT('',#5156);
#1637=VERTEX_POINT('',#5163);
#1638=VERTEX_POINT('',#5165);
#1639=VERTEX_POINT('',#5169);
#1640=VERTEX_POINT('',#5171);
#1641=VERTEX_POINT('',#5178);
#1642=VERTEX_POINT('',#5180);
#1643=VERTEX_POINT('',#5184);
#1644=VERTEX_POINT('',#5186);
#1645=VERTEX_POINT('',#5194);
#1646=VERTEX_POINT('',#5196);
#1647=VERTEX_POINT('',#5200);
#1648=VERTEX_POINT('',#5202);
#1649=VERTEX_POINT('',#5206);
#1650=VERTEX_POINT('',#5207);
#1651=VERTEX_POINT('',#5210);
#1652=VERTEX_POINT('',#5212);
#1653=VERTEX_POINT('',#5216);
#1654=VERTEX_POINT('',#5218);
#1655=VERTEX_POINT('',#5224);
#1656=VERTEX_POINT('',#5226);
#1657=VERTEX_POINT('',#5230);
#1658=VERTEX_POINT('',#5232);
#1659=VERTEX_POINT('',#5236);
#1660=VERTEX_POINT('',#5238);
#1661=VERTEX_POINT('',#5242);
#1662=VERTEX_POINT('',#5244);
#1663=VERTEX_POINT('',#5248);
#1664=VERTEX_POINT('',#5249);
#1665=VERTEX_POINT('',#5251);
#1666=VERTEX_POINT('',#5253);
#1667=VERTEX_POINT('',#5257);
#1668=VERTEX_POINT('',#5259);
#1669=VERTEX_POINT('',#5263);
#1670=VERTEX_POINT('',#5265);
#1671=VERTEX_POINT('',#5269);
#1672=VERTEX_POINT('',#5271);
#1673=VERTEX_POINT('',#5275);
#1674=VERTEX_POINT('',#5277);
#1675=VERTEX_POINT('',#5281);
#1676=VERTEX_POINT('',#5283);
#1677=VERTEX_POINT('',#5287);
#1678=VERTEX_POINT('',#5289);
#1679=VERTEX_POINT('',#5299);
#1680=VERTEX_POINT('',#5301);
#1681=VERTEX_POINT('',#5305);
#1682=VERTEX_POINT('',#5308);
#1683=VERTEX_POINT('',#5309);
#1684=VERTEX_POINT('',#5311);
#1685=VERTEX_POINT('',#5315);
#1686=VERTEX_POINT('',#5316);
#1687=VERTEX_POINT('',#5327);
#1688=VERTEX_POINT('',#5356);
#1689=VERTEX_POINT('',#5393);
#1690=VERTEX_POINT('',#5428);
#1691=VERTEX_POINT('',#5430);
#1692=VERTEX_POINT('',#5441);
#1693=VERTEX_POINT('',#5471);
#1694=VERTEX_POINT('',#5473);
#1695=VERTEX_POINT('',#5476);
#1696=VERTEX_POINT('',#5477);
#1697=VERTEX_POINT('',#5496);
#1698=VERTEX_POINT('',#5517);
#1699=VERTEX_POINT('',#5518);
#1700=VERTEX_POINT('',#5537);
#1701=VERTEX_POINT('',#5558);
#1702=VERTEX_POINT('',#5559);
#1703=VERTEX_POINT('',#5578);
#1704=VERTEX_POINT('',#5599);
#1705=VERTEX_POINT('',#5600);
#1706=VERTEX_POINT('',#5619);
#1707=VERTEX_POINT('',#5641);
#1708=VERTEX_POINT('',#5678);
#1709=VERTEX_POINT('',#5715);
#1710=VERTEX_POINT('',#5752);
#1711=VERTEX_POINT('',#5789);
#1712=VERTEX_POINT('',#5792);
#1713=VERTEX_POINT('',#5795);
#1714=VERTEX_POINT('',#5799);
#1715=VERTEX_POINT('',#5807);
#1716=VERTEX_POINT('',#5809);
#1717=VERTEX_POINT('',#5813);
#1718=VERTEX_POINT('',#5815);
#1719=VERTEX_POINT('',#5822);
#1720=VERTEX_POINT('',#5825);
#1721=VERTEX_POINT('',#5829);
#1722=VERTEX_POINT('',#5833);
#1723=VERTEX_POINT('',#5837);
#1724=VERTEX_POINT('',#5840);
#1725=VERTEX_POINT('',#5844);
#1726=VERTEX_POINT('',#5848);
#1727=VERTEX_POINT('',#5853);
#1728=VERTEX_POINT('',#5854);
#1729=VERTEX_POINT('',#5856);
#1730=VERTEX_POINT('',#5858);
#1731=VERTEX_POINT('',#5862);
#1732=VERTEX_POINT('',#5864);
#1733=VERTEX_POINT('',#5868);
#1734=VERTEX_POINT('',#5870);
#1735=VERTEX_POINT('',#5874);
#1736=VERTEX_POINT('',#5876);
#1737=VERTEX_POINT('',#5880);
#1738=VERTEX_POINT('',#5882);
#1739=VERTEX_POINT('',#5920);
#1740=VERTEX_POINT('',#5921);
#1741=VERTEX_POINT('',#5923);
#1742=VERTEX_POINT('',#5925);
#1743=VERTEX_POINT('',#5929);
#1744=VERTEX_POINT('',#5931);
#1745=VERTEX_POINT('',#5935);
#1746=VERTEX_POINT('',#5939);
#1747=VERTEX_POINT('',#5945);
#1748=VERTEX_POINT('',#5947);
#1749=VERTEX_POINT('',#5955);
#1750=VERTEX_POINT('',#5958);
#1751=VERTEX_POINT('',#5962);
#1752=VERTEX_POINT('',#5966);
#1753=VERTEX_POINT('',#5969);
#1754=VERTEX_POINT('',#5974);
#1755=VERTEX_POINT('',#5975);
#1756=VERTEX_POINT('',#6032);
#1757=VERTEX_POINT('',#6034);
#1758=VERTEX_POINT('',#6092);
#1759=VERTEX_POINT('',#6093);
#1760=VERTEX_POINT('',#6130);
#1761=VERTEX_POINT('',#6132);
#1762=VERTEX_POINT('',#6143);
#1763=VERTEX_POINT('',#6154);
#1764=VERTEX_POINT('',#6176);
#1765=VERTEX_POINT('',#6177);
#1766=VERTEX_POINT('',#6179);
#1767=VERTEX_POINT('',#6181);
#1768=VERTEX_POINT('',#6185);
#1769=VERTEX_POINT('',#6186);
#1770=VERTEX_POINT('',#6188);
#1771=VERTEX_POINT('',#6190);
#1772=VERTEX_POINT('',#6197);
#1773=VERTEX_POINT('',#6203);
#1774=VERTEX_POINT('',#6204);
#1775=VERTEX_POINT('',#6219);
#1776=VERTEX_POINT('',#6232);
#1777=VERTEX_POINT('',#6293);
#1778=VERTEX_POINT('',#6294);
#1779=VERTEX_POINT('',#6309);
#1780=VERTEX_POINT('',#6322);
#1781=VERTEX_POINT('',#6383);
#1782=VERTEX_POINT('',#6384);
#1783=VERTEX_POINT('',#6397);
#1784=VERTEX_POINT('',#6410);
#1785=VERTEX_POINT('',#6471);
#1786=VERTEX_POINT('',#6477);
#1787=VERTEX_POINT('',#6486);
#1788=VERTEX_POINT('',#6487);
#1789=VERTEX_POINT('',#6489);
#1790=VERTEX_POINT('',#6491);
#1791=VERTEX_POINT('',#6495);
#1792=VERTEX_POINT('',#6496);
#1793=VERTEX_POINT('',#6501);
#1794=VERTEX_POINT('',#6502);
#1795=VERTEX_POINT('',#6510);
#1796=VERTEX_POINT('',#6512);
#1797=VERTEX_POINT('',#6516);
#1798=VERTEX_POINT('',#6521);
#1799=VERTEX_POINT('',#6523);
#1800=VERTEX_POINT('',#6527);
#1801=VERTEX_POINT('',#6531);
#1802=VERTEX_POINT('',#6532);
#1803=VERTEX_POINT('',#6545);
#1804=VERTEX_POINT('',#6546);
#1805=VERTEX_POINT('',#6548);
#1806=VERTEX_POINT('',#6550);
#1807=VERTEX_POINT('',#6554);
#1808=VERTEX_POINT('',#6556);
#1809=VERTEX_POINT('',#6560);
#1810=VERTEX_POINT('',#6562);
#1811=VERTEX_POINT('',#6566);
#1812=VERTEX_POINT('',#6568);
#1813=VERTEX_POINT('',#6572);
#1814=VERTEX_POINT('',#6574);
#1815=VERTEX_POINT('',#6582);
#1816=VERTEX_POINT('',#6585);
#1817=VERTEX_POINT('',#6589);
#1818=VERTEX_POINT('',#6593);
#1819=VERTEX_POINT('',#6599);
#1820=VERTEX_POINT('',#6634);
#1821=VERTEX_POINT('',#6671);
#1822=VERTEX_POINT('',#6673);
#1823=VERTEX_POINT('',#6676);
#1824=VERTEX_POINT('',#6680);
#1825=VERTEX_POINT('',#6684);
#1826=VERTEX_POINT('',#6688);
#1827=VERTEX_POINT('',#6694);
#1828=VERTEX_POINT('',#6695);
#1829=VERTEX_POINT('',#6697);
#1830=VERTEX_POINT('',#6699);
#1831=VERTEX_POINT('',#6703);
#1832=VERTEX_POINT('',#6705);
#1833=VERTEX_POINT('',#6709);
#1834=VERTEX_POINT('',#6711);
#1835=VERTEX_POINT('',#6715);
#1836=VERTEX_POINT('',#6717);
#1837=VERTEX_POINT('',#6721);
#1838=VERTEX_POINT('',#6723);
#1839=VERTEX_POINT('',#6731);
#1840=VERTEX_POINT('',#6734);
#1841=VERTEX_POINT('',#6738);
#1842=VERTEX_POINT('',#6742);
#1843=EDGE_CURVE('',#1569,#1569,#1437,.T.);
#1844=EDGE_CURVE('',#1569,#1570,#981,.T.);
#1845=EDGE_CURVE('',#1570,#1570,#1438,.T.);
#1846=EDGE_CURVE('',#1571,#1571,#1439,.T.);
#1847=EDGE_CURVE('',#1571,#1572,#982,.T.);
#1848=EDGE_CURVE('',#1572,#1572,#1440,.T.);
#1849=EDGE_CURVE('',#1573,#1573,#1441,.T.);
#1850=EDGE_CURVE('',#1573,#1574,#983,.T.);
#1851=EDGE_CURVE('',#1574,#1574,#1442,.T.);
#1852=EDGE_CURVE('',#1575,#1575,#1443,.T.);
#1853=EDGE_CURVE('',#1575,#1576,#984,.T.);
#1854=EDGE_CURVE('',#1576,#1576,#1444,.T.);
#1855=EDGE_CURVE('',#1577,#1577,#1445,.T.);
#1856=EDGE_CURVE('',#1577,#1578,#985,.T.);
#1857=EDGE_CURVE('',#1578,#1578,#1446,.T.);
#1858=EDGE_CURVE('',#1579,#1580,#986,.T.);
#1859=EDGE_CURVE('',#1579,#1581,#987,.T.);
#1860=EDGE_CURVE('',#1582,#1581,#988,.T.);
#1861=EDGE_CURVE('',#1580,#1582,#989,.T.);
#1862=EDGE_CURVE('',#1583,#1584,#990,.T.);
#1863=EDGE_CURVE('',#1585,#1583,#991,.T.);
#1864=EDGE_CURVE('',#1586,#1585,#992,.T.);
#1865=EDGE_CURVE('',#1584,#1586,#993,.T.);
#1866=EDGE_CURVE('',#1584,#1579,#994,.T.);
#1867=EDGE_CURVE('',#1581,#1586,#995,.T.);
#1868=EDGE_CURVE('',#1582,#1585,#996,.T.);
#1869=EDGE_CURVE('',#1583,#1580,#997,.T.);
#1870=EDGE_CURVE('',#1587,#1587,#1447,.T.);
#1871=EDGE_CURVE('',#1587,#1588,#998,.T.);
#1872=EDGE_CURVE('',#1588,#1588,#1448,.T.);
#1873=EDGE_CURVE('',#1589,#1589,#1449,.T.);
#1874=EDGE_CURVE('',#1589,#1590,#999,.T.);
#1875=EDGE_CURVE('',#1590,#1590,#1450,.T.);
#1876=EDGE_CURVE('',#1591,#1591,#1451,.T.);
#1877=EDGE_CURVE('',#1591,#1592,#1000,.T.);
#1878=EDGE_CURVE('',#1592,#1592,#1452,.T.);
#1879=EDGE_CURVE('',#1593,#1593,#1453,.T.);
#1880=EDGE_CURVE('',#1593,#1594,#1001,.T.);
#1881=EDGE_CURVE('',#1594,#1594,#1454,.T.);
#1882=EDGE_CURVE('',#1595,#1595,#1455,.T.);
#1883=EDGE_CURVE('',#1595,#1596,#1002,.T.);
#1884=EDGE_CURVE('',#1596,#1596,#1456,.T.);
#1885=EDGE_CURVE('',#1597,#1598,#1003,.T.);
#1886=EDGE_CURVE('',#1597,#1599,#1004,.T.);
#1887=EDGE_CURVE('',#1600,#1599,#1005,.T.);
#1888=EDGE_CURVE('',#1598,#1600,#1006,.T.);
#1889=EDGE_CURVE('',#1601,#1602,#1007,.T.);
#1890=EDGE_CURVE('',#1603,#1601,#1008,.T.);
#1891=EDGE_CURVE('',#1604,#1603,#1009,.T.);
#1892=EDGE_CURVE('',#1602,#1604,#1010,.T.);
#1893=EDGE_CURVE('',#1602,#1597,#1011,.T.);
#1894=EDGE_CURVE('',#1599,#1604,#1012,.T.);
#1895=EDGE_CURVE('',#1600,#1603,#1013,.T.);
#1896=EDGE_CURVE('',#1601,#1598,#1014,.T.);
#1897=EDGE_CURVE('',#1605,#1606,#1015,.T.);
#1898=EDGE_CURVE('',#1606,#1607,#1016,.T.);
#1899=EDGE_CURVE('',#1608,#1607,#1017,.T.);
#1900=EDGE_CURVE('',#1605,#1608,#1018,.T.);
#1901=EDGE_CURVE('',#1609,#1605,#1019,.T.);
#1902=EDGE_CURVE('',#1610,#1608,#1020,.T.);
#1903=EDGE_CURVE('',#1609,#1610,#1021,.T.);
#1904=EDGE_CURVE('',#1611,#1609,#1022,.T.);
#1905=EDGE_CURVE('',#1612,#1610,#1023,.T.);
#1906=EDGE_CURVE('',#1611,#1612,#1024,.T.);
#1907=EDGE_CURVE('',#1606,#1611,#1025,.T.);
#1908=EDGE_CURVE('',#1607,#1612,#1026,.T.);
#1909=EDGE_CURVE('',#1613,#1613,#1457,.T.);
#1910=EDGE_CURVE('',#1613,#1614,#1027,.T.);
#1911=EDGE_CURVE('',#1614,#1614,#1458,.T.);
#1912=EDGE_CURVE('',#1615,#1615,#1459,.T.);
#1913=EDGE_CURVE('',#1615,#1616,#1028,.T.);
#1914=EDGE_CURVE('',#1616,#1616,#1460,.T.);
#1915=EDGE_CURVE('',#1617,#1617,#1461,.T.);
#1916=EDGE_CURVE('',#1617,#1618,#1029,.T.);
#1917=EDGE_CURVE('',#1618,#1618,#1462,.T.);
#1918=EDGE_CURVE('',#1619,#1619,#1463,.T.);
#1919=EDGE_CURVE('',#1619,#1620,#1030,.T.);
#1920=EDGE_CURVE('',#1620,#1620,#1464,.T.);
#1921=EDGE_CURVE('',#1621,#1621,#1465,.T.);
#1922=EDGE_CURVE('',#1621,#1622,#1031,.T.);
#1923=EDGE_CURVE('',#1622,#1622,#1466,.T.);
#1924=EDGE_CURVE('',#1623,#1623,#1467,.T.);
#1925=EDGE_CURVE('',#1623,#1624,#1032,.T.);
#1926=EDGE_CURVE('',#1624,#1624,#1468,.T.);
#1927=EDGE_CURVE('',#1625,#1625,#1469,.T.);
#1928=EDGE_CURVE('',#1625,#1626,#1033,.T.);
#1929=EDGE_CURVE('',#1626,#1626,#1470,.T.);
#1930=EDGE_CURVE('',#1627,#1627,#1471,.T.);
#1931=EDGE_CURVE('',#1627,#1628,#1034,.T.);
#1932=EDGE_CURVE('',#1628,#1628,#1472,.T.);
#1933=EDGE_CURVE('',#1629,#1629,#1473,.T.);
#1934=EDGE_CURVE('',#1629,#1630,#1035,.T.);
#1935=EDGE_CURVE('',#1630,#1630,#1474,.T.);
#1936=EDGE_CURVE('',#1631,#1631,#1475,.T.);
#1937=EDGE_CURVE('',#1631,#1632,#1036,.T.);
#1938=EDGE_CURVE('',#1632,#1632,#1476,.T.);
#1939=EDGE_CURVE('',#1633,#1633,#1477,.T.);
#1940=EDGE_CURVE('',#1633,#1634,#1037,.T.);
#1941=EDGE_CURVE('',#1634,#1634,#1478,.T.);
#1942=EDGE_CURVE('',#1635,#1635,#1479,.T.);
#1943=EDGE_CURVE('',#1635,#1636,#1038,.T.);
#1944=EDGE_CURVE('',#1636,#1636,#1480,.T.);
#1945=EDGE_CURVE('',#1637,#1637,#1481,.T.);
#1946=EDGE_CURVE('',#1637,#1638,#1039,.T.);
#1947=EDGE_CURVE('',#1638,#1638,#1482,.T.);
#1948=EDGE_CURVE('',#1639,#1639,#1483,.T.);
#1949=EDGE_CURVE('',#1639,#1640,#1040,.T.);
#1950=EDGE_CURVE('',#1640,#1640,#1484,.T.);
#1951=EDGE_CURVE('',#1641,#1641,#1485,.T.);
#1952=EDGE_CURVE('',#1641,#1642,#1041,.T.);
#1953=EDGE_CURVE('',#1642,#1642,#1486,.T.);
#1954=EDGE_CURVE('',#1643,#1643,#1487,.T.);
#1955=EDGE_CURVE('',#1643,#1644,#1042,.T.);
#1956=EDGE_CURVE('',#1644,#1644,#1488,.T.);
#1957=EDGE_CURVE('',#1645,#1645,#1489,.T.);
#1958=EDGE_CURVE('',#1645,#1646,#1043,.T.);
#1959=EDGE_CURVE('',#1646,#1646,#1490,.T.);
#1960=EDGE_CURVE('',#1647,#1647,#1491,.T.);
#1961=EDGE_CURVE('',#1647,#1648,#1044,.T.);
#1962=EDGE_CURVE('',#1648,#1648,#1492,.T.);
#1963=EDGE_CURVE('',#1649,#1650,#1493,.T.);
#1964=EDGE_CURVE('',#1651,#1651,#1494,.T.);
#1965=EDGE_CURVE('',#1651,#1652,#1045,.T.);
#1966=EDGE_CURVE('',#1652,#1652,#1495,.T.);
#1967=EDGE_CURVE('',#1653,#1653,#1496,.T.);
#1968=EDGE_CURVE('',#1653,#1654,#1046,.T.);
#1969=EDGE_CURVE('',#1654,#1654,#1497,.T.);
#1970=EDGE_CURVE('',#1655,#1655,#1498,.T.);
#1971=EDGE_CURVE('',#1655,#1656,#1047,.T.);
#1972=EDGE_CURVE('',#1656,#1656,#1499,.T.);
#1973=EDGE_CURVE('',#1657,#1657,#1500,.T.);
#1974=EDGE_CURVE('',#1657,#1658,#1048,.T.);
#1975=EDGE_CURVE('',#1658,#1658,#1501,.T.);
#1976=EDGE_CURVE('',#1659,#1659,#1502,.T.);
#1977=EDGE_CURVE('',#1659,#1660,#1049,.T.);
#1978=EDGE_CURVE('',#1660,#1660,#1503,.T.);
#1979=EDGE_CURVE('',#1661,#1661,#1504,.T.);
#1980=EDGE_CURVE('',#1661,#1662,#1050,.T.);
#1981=EDGE_CURVE('',#1662,#1662,#1505,.T.);
#1982=EDGE_CURVE('',#1663,#1664,#1051,.T.);
#1983=EDGE_CURVE('',#1664,#1665,#1052,.T.);
#1984=EDGE_CURVE('',#1666,#1665,#1053,.T.);
#1985=EDGE_CURVE('',#1663,#1666,#1054,.T.);
#1986=EDGE_CURVE('',#1667,#1663,#1055,.T.);
#1987=EDGE_CURVE('',#1668,#1666,#1056,.T.);
#1988=EDGE_CURVE('',#1667,#1668,#1057,.T.);
#1989=EDGE_CURVE('',#1669,#1667,#1058,.T.);
#1990=EDGE_CURVE('',#1670,#1668,#1059,.T.);
#1991=EDGE_CURVE('',#1669,#1670,#1060,.T.);
#1992=EDGE_CURVE('',#1671,#1669,#1061,.T.);
#1993=EDGE_CURVE('',#1672,#1670,#1062,.T.);
#1994=EDGE_CURVE('',#1671,#1672,#1063,.T.);
#1995=EDGE_CURVE('',#1673,#1671,#1064,.T.);
#1996=EDGE_CURVE('',#1674,#1672,#1065,.T.);
#1997=EDGE_CURVE('',#1673,#1674,#1066,.T.);
#1998=EDGE_CURVE('',#1675,#1673,#1067,.T.);
#1999=EDGE_CURVE('',#1676,#1674,#1068,.T.);
#2000=EDGE_CURVE('',#1675,#1676,#1069,.T.);
#2001=EDGE_CURVE('',#1677,#1675,#1070,.T.);
#2002=EDGE_CURVE('',#1678,#1676,#1071,.T.);
#2003=EDGE_CURVE('',#1677,#1678,#1072,.T.);
#2004=EDGE_CURVE('',#1664,#1677,#1073,.T.);
#2005=EDGE_CURVE('',#1665,#1678,#1074,.T.);
#2006=EDGE_CURVE('',#1679,#1679,#1506,.T.);
#2007=EDGE_CURVE('',#1679,#1680,#1075,.T.);
#2008=EDGE_CURVE('',#1680,#1680,#1507,.T.);
#2009=EDGE_CURVE('',#1681,#1681,#1508,.T.);
#2010=EDGE_CURVE('',#1682,#1683,#1509,.T.);
#2011=EDGE_CURVE('',#1684,#1684,#1510,.T.);
#2012=EDGE_CURVE('',#1685,#1686,#189,.T.);
#2013=EDGE_CURVE('',#1687,#1685,#190,.T.);
#2014=EDGE_CURVE('',#1686,#1687,#191,.T.);
#2015=EDGE_CURVE('',#1686,#1688,#1076,.T.);
#2016=EDGE_CURVE('',#1688,#1688,#192,.T.);
#2017=EDGE_CURVE('',#1689,#1689,#193,.T.);
#2018=EDGE_CURVE('',#1689,#1690,#1077,.T.);
#2019=EDGE_CURVE('',#1691,#1690,#194,.T.);
#2020=EDGE_CURVE('',#1692,#1691,#195,.T.);
#2021=EDGE_CURVE('',#1690,#1692,#196,.T.);
#2022=EDGE_CURVE('',#1693,#1693,#1511,.T.);
#2023=EDGE_CURVE('',#1693,#1694,#1078,.T.);
#2024=EDGE_CURVE('',#1694,#1694,#1512,.T.);
#2025=EDGE_CURVE('',#1695,#1696,#197,.T.);
#2026=EDGE_CURVE('',#1696,#1697,#198,.T.);
#2027=EDGE_CURVE('',#1697,#1695,#199,.T.);
#2028=EDGE_CURVE('',#1698,#1699,#200,.T.);
#2029=EDGE_CURVE('',#1699,#1700,#201,.T.);
#2030=EDGE_CURVE('',#1700,#1698,#202,.T.);
#2031=EDGE_CURVE('',#1701,#1702,#203,.T.);
#2032=EDGE_CURVE('',#1702,#1703,#204,.T.);
#2033=EDGE_CURVE('',#1703,#1701,#205,.T.);
#2034=EDGE_CURVE('',#1704,#1705,#206,.T.);
#2035=EDGE_CURVE('',#1705,#1706,#207,.T.);
#2036=EDGE_CURVE('',#1706,#1704,#208,.T.);
#2037=EDGE_CURVE('',#1697,#1707,#1079,.T.);
#2038=EDGE_CURVE('',#1707,#1707,#209,.T.);
#2039=EDGE_CURVE('',#1708,#1708,#210,.T.);
#2040=EDGE_CURVE('',#1708,#1700,#1080,.T.);
#2041=EDGE_CURVE('',#1703,#1709,#1081,.T.);
#2042=EDGE_CURVE('',#1709,#1709,#211,.T.);
#2043=EDGE_CURVE('',#1710,#1710,#212,.T.);
#2044=EDGE_CURVE('',#1710,#1706,#1082,.T.);
#2045=EDGE_CURVE('',#1711,#1711,#1513,.T.);
#2046=EDGE_CURVE('',#1712,#1712,#1514,.T.);
#2047=EDGE_CURVE('',#1713,#1713,#1515,.T.);
#2048=EDGE_CURVE('',#1713,#1712,#1083,.T.);
#2049=EDGE_CURVE('',#1714,#1714,#1516,.T.);
#2050=EDGE_CURVE('',#1714,#1711,#1084,.T.);
#2051=EDGE_CURVE('',#1715,#1715,#1517,.T.);
#2052=EDGE_CURVE('',#1715,#1716,#1085,.T.);
#2053=EDGE_CURVE('',#1716,#1716,#1518,.T.);
#2054=EDGE_CURVE('',#1717,#1717,#1519,.T.);
#2055=EDGE_CURVE('',#1717,#1718,#1086,.T.);
#2056=EDGE_CURVE('',#1718,#1718,#1520,.T.);
#2057=EDGE_CURVE('',#1719,#1719,#1521,.T.);
#2058=EDGE_CURVE('',#1720,#1720,#1522,.T.);
#2059=EDGE_CURVE('',#1720,#1719,#1087,.T.);
#2060=EDGE_CURVE('',#1721,#1721,#1523,.T.);
#2061=EDGE_CURVE('',#1721,#1720,#1088,.T.);
#2062=EDGE_CURVE('',#1722,#1722,#1524,.T.);
#2063=EDGE_CURVE('',#1722,#1721,#1089,.T.);
#2064=EDGE_CURVE('',#1723,#1723,#1525,.T.);
#2065=EDGE_CURVE('',#1724,#1724,#1526,.F.);
#2066=EDGE_CURVE('',#1724,#1723,#1090,.T.);
#2067=EDGE_CURVE('',#1725,#1725,#1527,.F.);
#2068=EDGE_CURVE('',#1725,#1724,#1091,.T.);
#2069=EDGE_CURVE('',#1726,#1726,#1528,.T.);
#2070=EDGE_CURVE('',#1726,#1725,#1092,.T.);
#2071=EDGE_CURVE('',#1727,#1728,#1093,.T.);
#2072=EDGE_CURVE('',#1728,#1729,#1094,.T.);
#2073=EDGE_CURVE('',#1729,#1730,#1095,.T.);
#2074=EDGE_CURVE('',#1727,#1730,#1096,.T.);
#2075=EDGE_CURVE('',#1728,#1731,#1097,.T.);
#2076=EDGE_CURVE('',#1731,#1732,#1098,.T.);
#2077=EDGE_CURVE('',#1732,#1729,#1099,.T.);
#2078=EDGE_CURVE('',#1731,#1733,#1100,.T.);
#2079=EDGE_CURVE('',#1733,#1734,#1101,.T.);
#2080=EDGE_CURVE('',#1734,#1732,#1102,.T.);
#2081=EDGE_CURVE('',#1733,#1735,#1103,.T.);
#2082=EDGE_CURVE('',#1735,#1736,#1104,.T.);
#2083=EDGE_CURVE('',#1736,#1734,#1105,.T.);
#2084=EDGE_CURVE('',#1735,#1737,#1106,.T.);
#2085=EDGE_CURVE('',#1737,#1738,#1107,.T.);
#2086=EDGE_CURVE('',#1738,#1736,#1108,.T.);
#2087=EDGE_CURVE('',#1737,#1727,#1109,.T.);
#2088=EDGE_CURVE('',#1730,#1738,#1110,.T.);
#2089=EDGE_CURVE('',#1739,#1740,#1111,.T.);
#2090=EDGE_CURVE('',#1739,#1741,#1112,.T.);
#2091=EDGE_CURVE('',#1741,#1742,#1113,.T.);
#2092=EDGE_CURVE('',#1742,#1740,#1114,.T.);
#2093=EDGE_CURVE('',#1740,#1743,#1529,.T.);
#2094=EDGE_CURVE('',#1744,#1742,#1115,.T.);
#2095=EDGE_CURVE('',#1743,#1744,#1116,.T.);
#2096=EDGE_CURVE('',#1741,#1745,#1117,.T.);
#2097=EDGE_CURVE('',#1745,#1744,#1118,.T.);
#2098=EDGE_CURVE('',#1743,#1746,#1119,.T.);
#2099=EDGE_CURVE('',#1745,#1746,#1120,.T.);
#2100=EDGE_CURVE('',#1746,#1739,#1530,.T.);
#2101=EDGE_CURVE('',#1747,#1747,#1531,.T.);
#2102=EDGE_CURVE('',#1747,#1748,#1121,.T.);
#2103=EDGE_CURVE('',#1748,#1748,#1532,.T.);
#2104=EDGE_CURVE('',#1749,#1749,#1533,.T.);
#2105=EDGE_CURVE('',#1750,#1750,#1534,.T.);
#2106=EDGE_CURVE('',#1750,#1749,#1122,.T.);
#2107=EDGE_CURVE('',#1751,#1751,#1535,.T.);
#2108=EDGE_CURVE('',#1751,#1750,#1123,.T.);
#2109=EDGE_CURVE('',#1752,#1752,#1536,.T.);
#2110=EDGE_CURVE('',#1753,#1753,#1537,.T.);
#2111=EDGE_CURVE('',#1753,#1752,#1124,.T.);
#2112=EDGE_CURVE('',#1754,#1755,#213,.T.);
#2113=EDGE_CURVE('',#1755,#1754,#214,.T.);
#2114=EDGE_CURVE('',#1755,#1756,#1125,.T.);
#2115=EDGE_CURVE('',#1757,#1756,#215,.T.);
#2116=EDGE_CURVE('',#1756,#1757,#216,.T.);
#2117=EDGE_CURVE('',#1758,#1759,#217,.T.);
#2118=EDGE_CURVE('',#1759,#1758,#218,.T.);
#2119=EDGE_CURVE('',#1759,#1760,#1126,.T.);
#2120=EDGE_CURVE('',#1761,#1760,#219,.T.);
#2121=EDGE_CURVE('',#1762,#1761,#220,.T.);
#2122=EDGE_CURVE('',#1763,#1762,#221,.T.);
#2123=EDGE_CURVE('',#1760,#1763,#222,.T.);
#2124=EDGE_CURVE('',#1764,#1765,#1127,.T.);
#2125=EDGE_CURVE('',#1764,#1766,#1128,.T.);
#2126=EDGE_CURVE('',#1767,#1766,#1129,.T.);
#2127=EDGE_CURVE('',#1765,#1767,#1130,.T.);
#2128=EDGE_CURVE('',#1768,#1769,#1131,.T.);
#2129=EDGE_CURVE('',#1770,#1768,#1132,.T.);
#2130=EDGE_CURVE('',#1771,#1770,#1133,.T.);
#2131=EDGE_CURVE('',#1771,#1769,#1134,.T.);
#2132=EDGE_CURVE('',#1769,#1764,#1135,.T.);
#2133=EDGE_CURVE('',#1766,#1771,#1136,.T.);
#2134=EDGE_CURVE('',#1772,#1772,#1538,.T.);
#2135=EDGE_CURVE('',#1767,#1770,#1539,.T.);
#2136=EDGE_CURVE('',#1765,#1768,#1540,.T.);
#2137=EDGE_CURVE('',#1773,#1774,#223,.T.);
#2138=EDGE_CURVE('',#1775,#1773,#224,.T.);
#2139=EDGE_CURVE('',#1775,#1776,#1137,.T.);
#2140=EDGE_CURVE('',#1776,#1776,#225,.T.);
#2141=EDGE_CURVE('',#1774,#1775,#226,.T.);
#2142=EDGE_CURVE('',#1777,#1778,#227,.T.);
#2143=EDGE_CURVE('',#1779,#1777,#228,.T.);
#2144=EDGE_CURVE('',#1779,#1780,#1138,.T.);
#2145=EDGE_CURVE('',#1780,#1780,#229,.T.);
#2146=EDGE_CURVE('',#1778,#1779,#230,.T.);
#2147=EDGE_CURVE('',#1781,#1782,#231,.T.);
#2148=EDGE_CURVE('',#1783,#1781,#232,.T.);
#2149=EDGE_CURVE('',#1783,#1784,#1139,.T.);
#2150=EDGE_CURVE('',#1784,#1784,#233,.T.);
#2151=EDGE_CURVE('',#1782,#1783,#234,.T.);
#2152=EDGE_CURVE('',#1785,#1785,#1541,.T.);
#2153=EDGE_CURVE('',#1772,#1763,#1140,.T.);
#2154=EDGE_CURVE('',#1761,#1785,#1141,.T.);
#2155=EDGE_CURVE('',#1786,#1786,#1542,.T.);
#2156=EDGE_CURVE('',#1774,#1786,#1543,.T.);
#2157=EDGE_CURVE('',#1778,#1775,#1544,.T.);
#2158=EDGE_CURVE('',#1782,#1779,#1545,.T.);
#2159=EDGE_CURVE('',#1786,#1783,#1546,.T.);
#2160=EDGE_CURVE('',#1787,#1788,#1142,.T.);
#2161=EDGE_CURVE('',#1788,#1789,#1143,.T.);
#2162=EDGE_CURVE('',#1789,#1790,#1144,.T.);
#2163=EDGE_CURVE('',#1790,#1787,#1145,.T.);
#2164=EDGE_CURVE('',#1791,#1792,#1146,.T.);
#2165=EDGE_CURVE('',#1792,#1788,#1547,.T.);
#2166=EDGE_CURVE('',#1787,#1791,#1548,.T.);
#2167=EDGE_CURVE('',#1793,#1794,#1147,.T.);
#2168=EDGE_CURVE('',#1794,#1792,#1148,.T.);
#2169=EDGE_CURVE('',#1791,#1793,#1149,.T.);
#2170=EDGE_CURVE('',#1789,#1794,#1549,.T.);
#2171=EDGE_CURVE('',#1793,#1790,#1550,.T.);
#2172=EDGE_CURVE('',#1795,#1787,#1150,.T.);
#2173=EDGE_CURVE('',#1796,#1795,#1551,.T.);
#2174=EDGE_CURVE('',#1796,#1791,#1151,.T.);
#2175=EDGE_CURVE('',#1797,#1790,#1152,.T.);
#2176=EDGE_CURVE('',#1795,#1797,#1153,.T.);
#2177=EDGE_CURVE('',#1798,#1795,#1154,.T.);
#2178=EDGE_CURVE('',#1797,#1799,#1155,.T.);
#2179=EDGE_CURVE('',#1799,#1798,#1156,.T.);
#2180=EDGE_CURVE('',#1800,#1796,#1157,.T.);
#2181=EDGE_CURVE('',#1798,#1800,#1552,.T.);
#2182=EDGE_CURVE('',#1801,#1802,#1158,.T.);
#2183=EDGE_CURVE('',#1802,#1796,#1159,.T.);
#2184=EDGE_CURVE('',#1800,#1801,#1160,.T.);
#2185=EDGE_CURVE('',#1797,#1802,#1553,.T.);
#2186=EDGE_CURVE('',#1801,#1799,#1554,.T.);
#2187=EDGE_CURVE('',#1802,#1793,#1161,.T.);
#2188=EDGE_CURVE('',#1803,#1804,#1162,.T.);
#2189=EDGE_CURVE('',#1803,#1805,#1163,.T.);
#2190=EDGE_CURVE('',#1805,#1806,#1164,.T.);
#2191=EDGE_CURVE('',#1804,#1806,#1165,.T.);
#2192=EDGE_CURVE('',#1807,#1803,#1166,.T.);
#2193=EDGE_CURVE('',#1807,#1808,#1167,.T.);
#2194=EDGE_CURVE('',#1808,#1805,#1168,.T.);
#2195=EDGE_CURVE('',#1809,#1807,#1169,.T.);
#2196=EDGE_CURVE('',#1809,#1810,#1170,.T.);
#2197=EDGE_CURVE('',#1810,#1808,#1171,.T.);
#2198=EDGE_CURVE('',#1811,#1809,#1172,.T.);
#2199=EDGE_CURVE('',#1811,#1812,#1173,.T.);
#2200=EDGE_CURVE('',#1812,#1810,#1174,.T.);
#2201=EDGE_CURVE('',#1813,#1811,#1175,.T.);
#2202=EDGE_CURVE('',#1813,#1814,#1176,.T.);
#2203=EDGE_CURVE('',#1814,#1812,#1177,.T.);
#2204=EDGE_CURVE('',#1804,#1813,#1178,.T.);
#2205=EDGE_CURVE('',#1806,#1814,#1179,.T.);
#2206=EDGE_CURVE('',#1815,#1815,#1555,.T.);
#2207=EDGE_CURVE('',#1816,#1816,#1556,.T.);
#2208=EDGE_CURVE('',#1816,#1815,#1180,.T.);
#2209=EDGE_CURVE('',#1817,#1817,#1557,.F.);
#2210=EDGE_CURVE('',#1817,#1816,#1181,.T.);
#2211=EDGE_CURVE('',#1818,#1818,#1558,.T.);
#2212=EDGE_CURVE('',#1818,#1817,#1182,.T.);
#2213=EDGE_CURVE('',#1819,#1819,#235,.T.);
#2214=EDGE_CURVE('',#1819,#1820,#1183,.T.);
#2215=EDGE_CURVE('',#1820,#1820,#236,.T.);
#2216=EDGE_CURVE('',#1821,#1821,#1559,.T.);
#2217=EDGE_CURVE('',#1822,#1822,#1560,.T.);
#2218=EDGE_CURVE('',#1823,#1823,#1561,.T.);
#2219=EDGE_CURVE('',#1823,#1821,#1184,.T.);
#2220=EDGE_CURVE('',#1824,#1824,#1562,.T.);
#2221=EDGE_CURVE('',#1824,#1823,#1185,.T.);
#2222=EDGE_CURVE('',#1825,#1825,#1563,.T.);
#2223=EDGE_CURVE('',#1825,#1824,#1186,.T.);
#2224=EDGE_CURVE('',#1826,#1826,#1564,.T.);
#2225=EDGE_CURVE('',#1826,#1822,#1187,.T.);
#2226=EDGE_CURVE('',#1827,#1828,#1188,.T.);
#2227=EDGE_CURVE('',#1827,#1829,#1189,.T.);
#2228=EDGE_CURVE('',#1829,#1830,#1190,.T.);
#2229=EDGE_CURVE('',#1828,#1830,#1191,.T.);
#2230=EDGE_CURVE('',#1831,#1827,#1192,.T.);
#2231=EDGE_CURVE('',#1831,#1832,#1193,.T.);
#2232=EDGE_CURVE('',#1832,#1829,#1194,.T.);
#2233=EDGE_CURVE('',#1833,#1831,#1195,.T.);
#2234=EDGE_CURVE('',#1833,#1834,#1196,.T.);
#2235=EDGE_CURVE('',#1834,#1832,#1197,.T.);
#2236=EDGE_CURVE('',#1835,#1833,#1198,.T.);
#2237=EDGE_CURVE('',#1835,#1836,#1199,.T.);
#2238=EDGE_CURVE('',#1836,#1834,#1200,.T.);
#2239=EDGE_CURVE('',#1837,#1835,#1201,.T.);
#2240=EDGE_CURVE('',#1837,#1838,#1202,.T.);
#2241=EDGE_CURVE('',#1838,#1836,#1203,.T.);
#2242=EDGE_CURVE('',#1828,#1837,#1204,.T.);
#2243=EDGE_CURVE('',#1830,#1838,#1205,.T.);
#2244=EDGE_CURVE('',#1839,#1839,#1565,.T.);
#2245=EDGE_CURVE('',#1840,#1840,#1566,.T.);
#2246=EDGE_CURVE('',#1840,#1839,#1206,.T.);
#2247=EDGE_CURVE('',#1841,#1841,#1567,.F.);
#2248=EDGE_CURVE('',#1841,#1840,#1207,.T.);
#2249=EDGE_CURVE('',#1842,#1842,#1568,.T.);
#2250=EDGE_CURVE('',#1842,#1841,#1208,.T.);
#2251=ORIENTED_EDGE('',*,*,#1843,.F.);
#2252=ORIENTED_EDGE('',*,*,#1844,.T.);
#2253=ORIENTED_EDGE('',*,*,#1845,.F.);
#2254=ORIENTED_EDGE('',*,*,#1844,.F.);
#2255=ORIENTED_EDGE('',*,*,#1846,.F.);
#2256=ORIENTED_EDGE('',*,*,#1847,.T.);
#2257=ORIENTED_EDGE('',*,*,#1848,.F.);
#2258=ORIENTED_EDGE('',*,*,#1847,.F.);
#2259=ORIENTED_EDGE('',*,*,#1849,.F.);
#2260=ORIENTED_EDGE('',*,*,#1850,.T.);
#2261=ORIENTED_EDGE('',*,*,#1851,.F.);
#2262=ORIENTED_EDGE('',*,*,#1850,.F.);
#2263=ORIENTED_EDGE('',*,*,#1852,.F.);
#2264=ORIENTED_EDGE('',*,*,#1853,.T.);
#2265=ORIENTED_EDGE('',*,*,#1854,.F.);
#2266=ORIENTED_EDGE('',*,*,#1853,.F.);
#2267=ORIENTED_EDGE('',*,*,#1855,.F.);
#2268=ORIENTED_EDGE('',*,*,#1856,.T.);
#2269=ORIENTED_EDGE('',*,*,#1857,.F.);
#2270=ORIENTED_EDGE('',*,*,#1856,.F.);
#2271=ORIENTED_EDGE('',*,*,#1858,.F.);
#2272=ORIENTED_EDGE('',*,*,#1859,.T.);
#2273=ORIENTED_EDGE('',*,*,#1860,.F.);
#2274=ORIENTED_EDGE('',*,*,#1861,.F.);
#2275=ORIENTED_EDGE('',*,*,#1862,.F.);
#2276=ORIENTED_EDGE('',*,*,#1863,.F.);
#2277=ORIENTED_EDGE('',*,*,#1864,.F.);
#2278=ORIENTED_EDGE('',*,*,#1865,.F.);
#2279=ORIENTED_EDGE('',*,*,#1866,.F.);
#2280=ORIENTED_EDGE('',*,*,#1865,.T.);
#2281=ORIENTED_EDGE('',*,*,#1867,.F.);
#2282=ORIENTED_EDGE('',*,*,#1859,.F.);
#2283=ORIENTED_EDGE('',*,*,#1867,.T.);
#2284=ORIENTED_EDGE('',*,*,#1864,.T.);
#2285=ORIENTED_EDGE('',*,*,#1868,.F.);
#2286=ORIENTED_EDGE('',*,*,#1860,.T.);
#2287=ORIENTED_EDGE('',*,*,#1857,.T.);
#2288=ORIENTED_EDGE('',*,*,#1854,.T.);
#2289=ORIENTED_EDGE('',*,*,#1851,.T.);
#2290=ORIENTED_EDGE('',*,*,#1848,.T.);
#2291=ORIENTED_EDGE('',*,*,#1845,.T.);
#2292=ORIENTED_EDGE('',*,*,#1866,.T.);
#2293=ORIENTED_EDGE('',*,*,#1858,.T.);
#2294=ORIENTED_EDGE('',*,*,#1869,.F.);
#2295=ORIENTED_EDGE('',*,*,#1862,.T.);
#2296=ORIENTED_EDGE('',*,*,#1855,.T.);
#2297=ORIENTED_EDGE('',*,*,#1852,.T.);
#2298=ORIENTED_EDGE('',*,*,#1849,.T.);
#2299=ORIENTED_EDGE('',*,*,#1846,.T.);
#2300=ORIENTED_EDGE('',*,*,#1843,.T.);
#2301=ORIENTED_EDGE('',*,*,#1870,.F.);
#2302=ORIENTED_EDGE('',*,*,#1871,.T.);
#2303=ORIENTED_EDGE('',*,*,#1872,.F.);
#2304=ORIENTED_EDGE('',*,*,#1871,.F.);
#2305=ORIENTED_EDGE('',*,*,#1873,.F.);
#2306=ORIENTED_EDGE('',*,*,#1874,.T.);
#2307=ORIENTED_EDGE('',*,*,#1875,.F.);
#2308=ORIENTED_EDGE('',*,*,#1874,.F.);
#2309=ORIENTED_EDGE('',*,*,#1876,.F.);
#2310=ORIENTED_EDGE('',*,*,#1877,.T.);
#2311=ORIENTED_EDGE('',*,*,#1878,.F.);
#2312=ORIENTED_EDGE('',*,*,#1877,.F.);
#2313=ORIENTED_EDGE('',*,*,#1879,.F.);
#2314=ORIENTED_EDGE('',*,*,#1880,.T.);
#2315=ORIENTED_EDGE('',*,*,#1881,.F.);
#2316=ORIENTED_EDGE('',*,*,#1880,.F.);
#2317=ORIENTED_EDGE('',*,*,#1882,.F.);
#2318=ORIENTED_EDGE('',*,*,#1883,.T.);
#2319=ORIENTED_EDGE('',*,*,#1884,.F.);
#2320=ORIENTED_EDGE('',*,*,#1883,.F.);
#2321=ORIENTED_EDGE('',*,*,#1885,.F.);
#2322=ORIENTED_EDGE('',*,*,#1886,.T.);
#2323=ORIENTED_EDGE('',*,*,#1887,.F.);
#2324=ORIENTED_EDGE('',*,*,#1888,.F.);
#2325=ORIENTED_EDGE('',*,*,#1889,.F.);
#2326=ORIENTED_EDGE('',*,*,#1890,.F.);
#2327=ORIENTED_EDGE('',*,*,#1891,.F.);
#2328=ORIENTED_EDGE('',*,*,#1892,.F.);
#2329=ORIENTED_EDGE('',*,*,#1893,.F.);
#2330=ORIENTED_EDGE('',*,*,#1892,.T.);
#2331=ORIENTED_EDGE('',*,*,#1894,.F.);
#2332=ORIENTED_EDGE('',*,*,#1886,.F.);
#2333=ORIENTED_EDGE('',*,*,#1894,.T.);
#2334=ORIENTED_EDGE('',*,*,#1891,.T.);
#2335=ORIENTED_EDGE('',*,*,#1895,.F.);
#2336=ORIENTED_EDGE('',*,*,#1887,.T.);
#2337=ORIENTED_EDGE('',*,*,#1884,.T.);
#2338=ORIENTED_EDGE('',*,*,#1881,.T.);
#2339=ORIENTED_EDGE('',*,*,#1878,.T.);
#2340=ORIENTED_EDGE('',*,*,#1875,.T.);
#2341=ORIENTED_EDGE('',*,*,#1872,.T.);
#2342=ORIENTED_EDGE('',*,*,#1893,.T.);
#2343=ORIENTED_EDGE('',*,*,#1885,.T.);
#2344=ORIENTED_EDGE('',*,*,#1896,.F.);
#2345=ORIENTED_EDGE('',*,*,#1889,.T.);
#2346=ORIENTED_EDGE('',*,*,#1882,.T.);
#2347=ORIENTED_EDGE('',*,*,#1879,.T.);
#2348=ORIENTED_EDGE('',*,*,#1876,.T.);
#2349=ORIENTED_EDGE('',*,*,#1873,.T.);
#2350=ORIENTED_EDGE('',*,*,#1870,.T.);
#2351=ORIENTED_EDGE('',*,*,#1897,.T.);
#2352=ORIENTED_EDGE('',*,*,#1898,.T.);
#2353=ORIENTED_EDGE('',*,*,#1899,.F.);
#2354=ORIENTED_EDGE('',*,*,#1900,.F.);
#2355=ORIENTED_EDGE('',*,*,#1901,.T.);
#2356=ORIENTED_EDGE('',*,*,#1900,.T.);
#2357=ORIENTED_EDGE('',*,*,#1902,.F.);
#2358=ORIENTED_EDGE('',*,*,#1903,.F.);
#2359=ORIENTED_EDGE('',*,*,#1904,.T.);
#2360=ORIENTED_EDGE('',*,*,#1903,.T.);
#2361=ORIENTED_EDGE('',*,*,#1905,.F.);
#2362=ORIENTED_EDGE('',*,*,#1906,.F.);
#2363=ORIENTED_EDGE('',*,*,#1907,.T.);
#2364=ORIENTED_EDGE('',*,*,#1906,.T.);
#2365=ORIENTED_EDGE('',*,*,#1908,.F.);
#2366=ORIENTED_EDGE('',*,*,#1898,.F.);
#2367=ORIENTED_EDGE('',*,*,#1908,.T.);
#2368=ORIENTED_EDGE('',*,*,#1905,.T.);
#2369=ORIENTED_EDGE('',*,*,#1902,.T.);
#2370=ORIENTED_EDGE('',*,*,#1899,.T.);
#2371=ORIENTED_EDGE('',*,*,#1863,.T.);
#2372=ORIENTED_EDGE('',*,*,#1869,.T.);
#2373=ORIENTED_EDGE('',*,*,#1861,.T.);
#2374=ORIENTED_EDGE('',*,*,#1868,.T.);
#2375=ORIENTED_EDGE('',*,*,#1890,.T.);
#2376=ORIENTED_EDGE('',*,*,#1896,.T.);
#2377=ORIENTED_EDGE('',*,*,#1888,.T.);
#2378=ORIENTED_EDGE('',*,*,#1895,.T.);
#2379=ORIENTED_EDGE('',*,*,#1907,.F.);
#2380=ORIENTED_EDGE('',*,*,#1897,.F.);
#2381=ORIENTED_EDGE('',*,*,#1901,.F.);
#2382=ORIENTED_EDGE('',*,*,#1904,.F.);
#2383=ORIENTED_EDGE('',*,*,#1909,.F.);
#2384=ORIENTED_EDGE('',*,*,#1910,.T.);
#2385=ORIENTED_EDGE('',*,*,#1911,.T.);
#2386=ORIENTED_EDGE('',*,*,#1910,.F.);
#2387=ORIENTED_EDGE('',*,*,#1912,.F.);
#2388=ORIENTED_EDGE('',*,*,#1913,.T.);
#2389=ORIENTED_EDGE('',*,*,#1914,.T.);
#2390=ORIENTED_EDGE('',*,*,#1913,.F.);
#2391=ORIENTED_EDGE('',*,*,#1912,.T.);
#2392=ORIENTED_EDGE('',*,*,#1909,.T.);
#2393=ORIENTED_EDGE('',*,*,#1914,.F.);
#2394=ORIENTED_EDGE('',*,*,#1911,.F.);
#2395=ORIENTED_EDGE('',*,*,#1915,.F.);
#2396=ORIENTED_EDGE('',*,*,#1916,.T.);
#2397=ORIENTED_EDGE('',*,*,#1917,.T.);
#2398=ORIENTED_EDGE('',*,*,#1916,.F.);
#2399=ORIENTED_EDGE('',*,*,#1918,.F.);
#2400=ORIENTED_EDGE('',*,*,#1919,.T.);
#2401=ORIENTED_EDGE('',*,*,#1920,.T.);
#2402=ORIENTED_EDGE('',*,*,#1919,.F.);
#2403=ORIENTED_EDGE('',*,*,#1918,.T.);
#2404=ORIENTED_EDGE('',*,*,#1915,.T.);
#2405=ORIENTED_EDGE('',*,*,#1920,.F.);
#2406=ORIENTED_EDGE('',*,*,#1917,.F.);
#2407=ORIENTED_EDGE('',*,*,#1921,.F.);
#2408=ORIENTED_EDGE('',*,*,#1922,.T.);
#2409=ORIENTED_EDGE('',*,*,#1923,.T.);
#2410=ORIENTED_EDGE('',*,*,#1922,.F.);
#2411=ORIENTED_EDGE('',*,*,#1924,.F.);
#2412=ORIENTED_EDGE('',*,*,#1925,.T.);
#2413=ORIENTED_EDGE('',*,*,#1926,.T.);
#2414=ORIENTED_EDGE('',*,*,#1925,.F.);
#2415=ORIENTED_EDGE('',*,*,#1924,.T.);
#2416=ORIENTED_EDGE('',*,*,#1921,.T.);
#2417=ORIENTED_EDGE('',*,*,#1926,.F.);
#2418=ORIENTED_EDGE('',*,*,#1923,.F.);
#2419=ORIENTED_EDGE('',*,*,#1927,.F.);
#2420=ORIENTED_EDGE('',*,*,#1928,.T.);
#2421=ORIENTED_EDGE('',*,*,#1929,.T.);
#2422=ORIENTED_EDGE('',*,*,#1928,.F.);
#2423=ORIENTED_EDGE('',*,*,#1930,.F.);
#2424=ORIENTED_EDGE('',*,*,#1931,.T.);
#2425=ORIENTED_EDGE('',*,*,#1932,.T.);
#2426=ORIENTED_EDGE('',*,*,#1931,.F.);
#2427=ORIENTED_EDGE('',*,*,#1930,.T.);
#2428=ORIENTED_EDGE('',*,*,#1927,.T.);
#2429=ORIENTED_EDGE('',*,*,#1932,.F.);
#2430=ORIENTED_EDGE('',*,*,#1929,.F.);
#2431=ORIENTED_EDGE('',*,*,#1933,.F.);
#2432=ORIENTED_EDGE('',*,*,#1934,.T.);
#2433=ORIENTED_EDGE('',*,*,#1935,.T.);
#2434=ORIENTED_EDGE('',*,*,#1934,.F.);
#2435=ORIENTED_EDGE('',*,*,#1936,.F.);
#2436=ORIENTED_EDGE('',*,*,#1937,.T.);
#2437=ORIENTED_EDGE('',*,*,#1938,.T.);
#2438=ORIENTED_EDGE('',*,*,#1937,.F.);
#2439=ORIENTED_EDGE('',*,*,#1936,.T.);
#2440=ORIENTED_EDGE('',*,*,#1933,.T.);
#2441=ORIENTED_EDGE('',*,*,#1938,.F.);
#2442=ORIENTED_EDGE('',*,*,#1935,.F.);
#2443=ORIENTED_EDGE('',*,*,#1939,.F.);
#2444=ORIENTED_EDGE('',*,*,#1940,.T.);
#2445=ORIENTED_EDGE('',*,*,#1941,.T.);
#2446=ORIENTED_EDGE('',*,*,#1940,.F.);
#2447=ORIENTED_EDGE('',*,*,#1942,.F.);
#2448=ORIENTED_EDGE('',*,*,#1943,.T.);
#2449=ORIENTED_EDGE('',*,*,#1944,.T.);
#2450=ORIENTED_EDGE('',*,*,#1943,.F.);
#2451=ORIENTED_EDGE('',*,*,#1942,.T.);
#2452=ORIENTED_EDGE('',*,*,#1939,.T.);
#2453=ORIENTED_EDGE('',*,*,#1944,.F.);
#2454=ORIENTED_EDGE('',*,*,#1941,.F.);
#2455=ORIENTED_EDGE('',*,*,#1945,.F.);
#2456=ORIENTED_EDGE('',*,*,#1946,.T.);
#2457=ORIENTED_EDGE('',*,*,#1947,.T.);
#2458=ORIENTED_EDGE('',*,*,#1946,.F.);
#2459=ORIENTED_EDGE('',*,*,#1948,.F.);
#2460=ORIENTED_EDGE('',*,*,#1949,.T.);
#2461=ORIENTED_EDGE('',*,*,#1950,.T.);
#2462=ORIENTED_EDGE('',*,*,#1949,.F.);
#2463=ORIENTED_EDGE('',*,*,#1948,.T.);
#2464=ORIENTED_EDGE('',*,*,#1945,.T.);
#2465=ORIENTED_EDGE('',*,*,#1950,.F.);
#2466=ORIENTED_EDGE('',*,*,#1947,.F.);
#2467=ORIENTED_EDGE('',*,*,#1951,.F.);
#2468=ORIENTED_EDGE('',*,*,#1952,.T.);
#2469=ORIENTED_EDGE('',*,*,#1953,.T.);
#2470=ORIENTED_EDGE('',*,*,#1952,.F.);
#2471=ORIENTED_EDGE('',*,*,#1954,.F.);
#2472=ORIENTED_EDGE('',*,*,#1955,.T.);
#2473=ORIENTED_EDGE('',*,*,#1956,.T.);
#2474=ORIENTED_EDGE('',*,*,#1955,.F.);
#2475=ORIENTED_EDGE('',*,*,#1954,.T.);
#2476=ORIENTED_EDGE('',*,*,#1951,.T.);
#2477=ORIENTED_EDGE('',*,*,#1956,.F.);
#2478=ORIENTED_EDGE('',*,*,#1953,.F.);
#2479=ORIENTED_EDGE('',*,*,#1957,.F.);
#2480=ORIENTED_EDGE('',*,*,#1958,.T.);
#2481=ORIENTED_EDGE('',*,*,#1959,.F.);
#2482=ORIENTED_EDGE('',*,*,#1958,.F.);
#2483=ORIENTED_EDGE('',*,*,#1960,.F.);
#2484=ORIENTED_EDGE('',*,*,#1961,.T.);
#2485=ORIENTED_EDGE('',*,*,#1962,.F.);
#2486=ORIENTED_EDGE('',*,*,#1961,.F.);
#2487=ORIENTED_EDGE('',*,*,#1963,.T.);
#2488=ORIENTED_EDGE('',*,*,#1963,.F.);
#2489=ORIENTED_EDGE('',*,*,#1960,.T.);
#2490=ORIENTED_EDGE('',*,*,#1959,.T.);
#2491=ORIENTED_EDGE('',*,*,#1964,.F.);
#2492=ORIENTED_EDGE('',*,*,#1965,.T.);
#2493=ORIENTED_EDGE('',*,*,#1966,.F.);
#2494=ORIENTED_EDGE('',*,*,#1965,.F.);
#2495=ORIENTED_EDGE('',*,*,#1967,.F.);
#2496=ORIENTED_EDGE('',*,*,#1968,.T.);
#2497=ORIENTED_EDGE('',*,*,#1969,.F.);
#2498=ORIENTED_EDGE('',*,*,#1968,.F.);
#2499=ORIENTED_EDGE('',*,*,#1966,.T.);
#2500=ORIENTED_EDGE('',*,*,#1957,.T.);
#2501=ORIENTED_EDGE('',*,*,#1967,.T.);
#2502=ORIENTED_EDGE('',*,*,#1962,.T.);
#2503=ORIENTED_EDGE('',*,*,#1970,.F.);
#2504=ORIENTED_EDGE('',*,*,#1971,.T.);
#2505=ORIENTED_EDGE('',*,*,#1972,.F.);
#2506=ORIENTED_EDGE('',*,*,#1971,.F.);
#2507=ORIENTED_EDGE('',*,*,#1973,.F.);
#2508=ORIENTED_EDGE('',*,*,#1974,.T.);
#2509=ORIENTED_EDGE('',*,*,#1975,.F.);
#2510=ORIENTED_EDGE('',*,*,#1974,.F.);
#2511=ORIENTED_EDGE('',*,*,#1976,.F.);
#2512=ORIENTED_EDGE('',*,*,#1977,.T.);
#2513=ORIENTED_EDGE('',*,*,#1978,.F.);
#2514=ORIENTED_EDGE('',*,*,#1977,.F.);
#2515=ORIENTED_EDGE('',*,*,#1979,.F.);
#2516=ORIENTED_EDGE('',*,*,#1980,.T.);
#2517=ORIENTED_EDGE('',*,*,#1981,.F.);
#2518=ORIENTED_EDGE('',*,*,#1980,.F.);
#2519=ORIENTED_EDGE('',*,*,#1982,.T.);
#2520=ORIENTED_EDGE('',*,*,#1983,.T.);
#2521=ORIENTED_EDGE('',*,*,#1984,.F.);
#2522=ORIENTED_EDGE('',*,*,#1985,.F.);
#2523=ORIENTED_EDGE('',*,*,#1986,.T.);
#2524=ORIENTED_EDGE('',*,*,#1985,.T.);
#2525=ORIENTED_EDGE('',*,*,#1987,.F.);
#2526=ORIENTED_EDGE('',*,*,#1988,.F.);
#2527=ORIENTED_EDGE('',*,*,#1989,.T.);
#2528=ORIENTED_EDGE('',*,*,#1988,.T.);
#2529=ORIENTED_EDGE('',*,*,#1990,.F.);
#2530=ORIENTED_EDGE('',*,*,#1991,.F.);
#2531=ORIENTED_EDGE('',*,*,#1992,.T.);
#2532=ORIENTED_EDGE('',*,*,#1991,.T.);
#2533=ORIENTED_EDGE('',*,*,#1993,.F.);
#2534=ORIENTED_EDGE('',*,*,#1994,.F.);
#2535=ORIENTED_EDGE('',*,*,#1995,.T.);
#2536=ORIENTED_EDGE('',*,*,#1994,.T.);
#2537=ORIENTED_EDGE('',*,*,#1996,.F.);
#2538=ORIENTED_EDGE('',*,*,#1997,.F.);
#2539=ORIENTED_EDGE('',*,*,#1998,.T.);
#2540=ORIENTED_EDGE('',*,*,#1997,.T.);
#2541=ORIENTED_EDGE('',*,*,#1999,.F.);
#2542=ORIENTED_EDGE('',*,*,#2000,.F.);
#2543=ORIENTED_EDGE('',*,*,#2001,.T.);
#2544=ORIENTED_EDGE('',*,*,#2000,.T.);
#2545=ORIENTED_EDGE('',*,*,#2002,.F.);
#2546=ORIENTED_EDGE('',*,*,#2003,.F.);
#2547=ORIENTED_EDGE('',*,*,#2004,.T.);
#2548=ORIENTED_EDGE('',*,*,#2003,.T.);
#2549=ORIENTED_EDGE('',*,*,#2005,.F.);
#2550=ORIENTED_EDGE('',*,*,#1983,.F.);
#2551=ORIENTED_EDGE('',*,*,#2005,.T.);
#2552=ORIENTED_EDGE('',*,*,#2002,.T.);
#2553=ORIENTED_EDGE('',*,*,#1999,.T.);
#2554=ORIENTED_EDGE('',*,*,#1996,.T.);
#2555=ORIENTED_EDGE('',*,*,#1993,.T.);
#2556=ORIENTED_EDGE('',*,*,#1990,.T.);
#2557=ORIENTED_EDGE('',*,*,#1987,.T.);
#2558=ORIENTED_EDGE('',*,*,#1984,.T.);
#2559=ORIENTED_EDGE('',*,*,#1969,.T.);
#2560=ORIENTED_EDGE('',*,*,#1972,.T.);
#2561=ORIENTED_EDGE('',*,*,#1975,.T.);
#2562=ORIENTED_EDGE('',*,*,#1978,.T.);
#2563=ORIENTED_EDGE('',*,*,#1981,.T.);
#2564=ORIENTED_EDGE('',*,*,#2004,.F.);
#2565=ORIENTED_EDGE('',*,*,#1982,.F.);
#2566=ORIENTED_EDGE('',*,*,#1986,.F.);
#2567=ORIENTED_EDGE('',*,*,#1989,.F.);
#2568=ORIENTED_EDGE('',*,*,#1992,.F.);
#2569=ORIENTED_EDGE('',*,*,#1995,.F.);
#2570=ORIENTED_EDGE('',*,*,#1998,.F.);
#2571=ORIENTED_EDGE('',*,*,#2001,.F.);
#2572=ORIENTED_EDGE('',*,*,#1964,.T.);
#2573=ORIENTED_EDGE('',*,*,#1970,.T.);
#2574=ORIENTED_EDGE('',*,*,#1973,.T.);
#2575=ORIENTED_EDGE('',*,*,#1976,.T.);
#2576=ORIENTED_EDGE('',*,*,#1979,.T.);
#2577=ORIENTED_EDGE('',*,*,#2006,.T.);
#2578=ORIENTED_EDGE('',*,*,#2007,.T.);
#2579=ORIENTED_EDGE('',*,*,#2008,.F.);
#2580=ORIENTED_EDGE('',*,*,#2007,.F.);
#2581=ORIENTED_EDGE('',*,*,#2009,.F.);
#2582=ORIENTED_EDGE('',*,*,#2008,.T.);
#2583=ORIENTED_EDGE('',*,*,#2010,.T.);
#2584=ORIENTED_EDGE('',*,*,#2010,.F.);
#2585=ORIENTED_EDGE('',*,*,#2009,.T.);
#2586=ORIENTED_EDGE('',*,*,#2011,.F.);
#2587=ORIENTED_EDGE('',*,*,#2011,.T.);
#2588=ORIENTED_EDGE('',*,*,#2006,.F.);
#2589=ORIENTED_EDGE('',*,*,#2012,.F.);
#2590=ORIENTED_EDGE('',*,*,#2013,.F.);
#2591=ORIENTED_EDGE('',*,*,#2014,.F.);
#2592=ORIENTED_EDGE('',*,*,#2015,.T.);
#2593=ORIENTED_EDGE('',*,*,#2016,.F.);
#2594=ORIENTED_EDGE('',*,*,#2015,.F.);
#2595=ORIENTED_EDGE('',*,*,#2017,.F.);
#2596=ORIENTED_EDGE('',*,*,#2018,.T.);
#2597=ORIENTED_EDGE('',*,*,#2019,.F.);
#2598=ORIENTED_EDGE('',*,*,#2020,.F.);
#2599=ORIENTED_EDGE('',*,*,#2021,.F.);
#2600=ORIENTED_EDGE('',*,*,#2018,.F.);
#2601=ORIENTED_EDGE('',*,*,#2022,.F.);
#2602=ORIENTED_EDGE('',*,*,#2023,.T.);
#2603=ORIENTED_EDGE('',*,*,#2024,.T.);
#2604=ORIENTED_EDGE('',*,*,#2023,.F.);
#2605=ORIENTED_EDGE('',*,*,#2013,.T.);
#2606=ORIENTED_EDGE('',*,*,#2012,.T.);
#2607=ORIENTED_EDGE('',*,*,#2014,.T.);
#2608=ORIENTED_EDGE('',*,*,#2020,.T.);
#2609=ORIENTED_EDGE('',*,*,#2019,.T.);
#2610=ORIENTED_EDGE('',*,*,#2021,.T.);
#2611=ORIENTED_EDGE('',*,*,#2025,.T.);
#2612=ORIENTED_EDGE('',*,*,#2026,.T.);
#2613=ORIENTED_EDGE('',*,*,#2027,.T.);
#2614=ORIENTED_EDGE('',*,*,#2028,.T.);
#2615=ORIENTED_EDGE('',*,*,#2029,.T.);
#2616=ORIENTED_EDGE('',*,*,#2030,.T.);
#2617=ORIENTED_EDGE('',*,*,#2031,.T.);
#2618=ORIENTED_EDGE('',*,*,#2032,.T.);
#2619=ORIENTED_EDGE('',*,*,#2033,.T.);
#2620=ORIENTED_EDGE('',*,*,#2034,.T.);
#2621=ORIENTED_EDGE('',*,*,#2035,.T.);
#2622=ORIENTED_EDGE('',*,*,#2036,.T.);
#2623=ORIENTED_EDGE('',*,*,#2026,.F.);
#2624=ORIENTED_EDGE('',*,*,#2025,.F.);
#2625=ORIENTED_EDGE('',*,*,#2027,.F.);
#2626=ORIENTED_EDGE('',*,*,#2037,.T.);
#2627=ORIENTED_EDGE('',*,*,#2038,.F.);
#2628=ORIENTED_EDGE('',*,*,#2037,.F.);
#2629=ORIENTED_EDGE('',*,*,#2039,.F.);
#2630=ORIENTED_EDGE('',*,*,#2040,.T.);
#2631=ORIENTED_EDGE('',*,*,#2029,.F.);
#2632=ORIENTED_EDGE('',*,*,#2028,.F.);
#2633=ORIENTED_EDGE('',*,*,#2030,.F.);
#2634=ORIENTED_EDGE('',*,*,#2040,.F.);
#2635=ORIENTED_EDGE('',*,*,#2032,.F.);
#2636=ORIENTED_EDGE('',*,*,#2031,.F.);
#2637=ORIENTED_EDGE('',*,*,#2033,.F.);
#2638=ORIENTED_EDGE('',*,*,#2041,.T.);
#2639=ORIENTED_EDGE('',*,*,#2042,.F.);
#2640=ORIENTED_EDGE('',*,*,#2041,.F.);
#2641=ORIENTED_EDGE('',*,*,#2043,.F.);
#2642=ORIENTED_EDGE('',*,*,#2044,.T.);
#2643=ORIENTED_EDGE('',*,*,#2035,.F.);
#2644=ORIENTED_EDGE('',*,*,#2034,.F.);
#2645=ORIENTED_EDGE('',*,*,#2036,.F.);
#2646=ORIENTED_EDGE('',*,*,#2044,.F.);
#2647=ORIENTED_EDGE('',*,*,#2024,.F.);
#2648=ORIENTED_EDGE('',*,*,#2045,.T.);
#2649=ORIENTED_EDGE('',*,*,#2046,.F.);
#2650=ORIENTED_EDGE('',*,*,#2022,.T.);
#2651=ORIENTED_EDGE('',*,*,#2047,.F.);
#2652=ORIENTED_EDGE('',*,*,#2048,.T.);
#2653=ORIENTED_EDGE('',*,*,#2046,.T.);
#2654=ORIENTED_EDGE('',*,*,#2048,.F.);
#2655=ORIENTED_EDGE('',*,*,#2047,.T.);
#2656=ORIENTED_EDGE('',*,*,#2049,.F.);
#2657=ORIENTED_EDGE('',*,*,#2049,.T.);
#2658=ORIENTED_EDGE('',*,*,#2050,.T.);
#2659=ORIENTED_EDGE('',*,*,#2045,.F.);
#2660=ORIENTED_EDGE('',*,*,#2050,.F.);
#2661=ORIENTED_EDGE('',*,*,#2017,.T.);
#2662=ORIENTED_EDGE('',*,*,#2016,.T.);
#2663=ORIENTED_EDGE('',*,*,#2039,.T.);
#2664=ORIENTED_EDGE('',*,*,#2038,.T.);
#2665=ORIENTED_EDGE('',*,*,#2043,.T.);
#2666=ORIENTED_EDGE('',*,*,#2042,.T.);
#2667=ORIENTED_EDGE('',*,*,#2051,.F.);
#2668=ORIENTED_EDGE('',*,*,#2052,.T.);
#2669=ORIENTED_EDGE('',*,*,#2053,.T.);
#2670=ORIENTED_EDGE('',*,*,#2052,.F.);
#2671=ORIENTED_EDGE('',*,*,#2054,.F.);
#2672=ORIENTED_EDGE('',*,*,#2055,.T.);
#2673=ORIENTED_EDGE('',*,*,#2056,.T.);
#2674=ORIENTED_EDGE('',*,*,#2055,.F.);
#2675=ORIENTED_EDGE('',*,*,#2054,.T.);
#2676=ORIENTED_EDGE('',*,*,#2051,.T.);
#2677=ORIENTED_EDGE('',*,*,#2056,.F.);
#2678=ORIENTED_EDGE('',*,*,#2053,.F.);
#2679=ORIENTED_EDGE('',*,*,#2057,.F.);
#2680=ORIENTED_EDGE('',*,*,#2058,.F.);
#2681=ORIENTED_EDGE('',*,*,#2059,.T.);
#2682=ORIENTED_EDGE('',*,*,#2057,.T.);
#2683=ORIENTED_EDGE('',*,*,#2059,.F.);
#2684=ORIENTED_EDGE('',*,*,#2060,.F.);
#2685=ORIENTED_EDGE('',*,*,#2061,.T.);
#2686=ORIENTED_EDGE('',*,*,#2058,.T.);
#2687=ORIENTED_EDGE('',*,*,#2061,.F.);
#2688=ORIENTED_EDGE('',*,*,#2062,.F.);
#2689=ORIENTED_EDGE('',*,*,#2063,.T.);
#2690=ORIENTED_EDGE('',*,*,#2060,.T.);
#2691=ORIENTED_EDGE('',*,*,#2063,.F.);
#2692=ORIENTED_EDGE('',*,*,#2062,.T.);
#2693=ORIENTED_EDGE('',*,*,#2064,.F.);
#2694=ORIENTED_EDGE('',*,*,#2065,.F.);
#2695=ORIENTED_EDGE('',*,*,#2066,.T.);
#2696=ORIENTED_EDGE('',*,*,#2064,.T.);
#2697=ORIENTED_EDGE('',*,*,#2066,.F.);
#2698=ORIENTED_EDGE('',*,*,#2067,.F.);
#2699=ORIENTED_EDGE('',*,*,#2068,.T.);
#2700=ORIENTED_EDGE('',*,*,#2065,.T.);
#2701=ORIENTED_EDGE('',*,*,#2068,.F.);
#2702=ORIENTED_EDGE('',*,*,#2069,.F.);
#2703=ORIENTED_EDGE('',*,*,#2070,.T.);
#2704=ORIENTED_EDGE('',*,*,#2067,.T.);
#2705=ORIENTED_EDGE('',*,*,#2070,.F.);
#2706=ORIENTED_EDGE('',*,*,#2069,.T.);
#2707=ORIENTED_EDGE('',*,*,#2071,.T.);
#2708=ORIENTED_EDGE('',*,*,#2072,.T.);
#2709=ORIENTED_EDGE('',*,*,#2073,.T.);
#2710=ORIENTED_EDGE('',*,*,#2074,.F.);
#2711=ORIENTED_EDGE('',*,*,#2075,.T.);
#2712=ORIENTED_EDGE('',*,*,#2076,.T.);
#2713=ORIENTED_EDGE('',*,*,#2077,.T.);
#2714=ORIENTED_EDGE('',*,*,#2072,.F.);
#2715=ORIENTED_EDGE('',*,*,#2078,.T.);
#2716=ORIENTED_EDGE('',*,*,#2079,.T.);
#2717=ORIENTED_EDGE('',*,*,#2080,.T.);
#2718=ORIENTED_EDGE('',*,*,#2076,.F.);
#2719=ORIENTED_EDGE('',*,*,#2081,.T.);
#2720=ORIENTED_EDGE('',*,*,#2082,.T.);
#2721=ORIENTED_EDGE('',*,*,#2083,.T.);
#2722=ORIENTED_EDGE('',*,*,#2079,.F.);
#2723=ORIENTED_EDGE('',*,*,#2084,.T.);
#2724=ORIENTED_EDGE('',*,*,#2085,.T.);
#2725=ORIENTED_EDGE('',*,*,#2086,.T.);
#2726=ORIENTED_EDGE('',*,*,#2082,.F.);
#2727=ORIENTED_EDGE('',*,*,#2087,.T.);
#2728=ORIENTED_EDGE('',*,*,#2074,.T.);
#2729=ORIENTED_EDGE('',*,*,#2088,.T.);
#2730=ORIENTED_EDGE('',*,*,#2085,.F.);
#2731=ORIENTED_EDGE('',*,*,#2087,.F.);
#2732=ORIENTED_EDGE('',*,*,#2084,.F.);
#2733=ORIENTED_EDGE('',*,*,#2081,.F.);
#2734=ORIENTED_EDGE('',*,*,#2078,.F.);
#2735=ORIENTED_EDGE('',*,*,#2075,.F.);
#2736=ORIENTED_EDGE('',*,*,#2071,.F.);
#2737=ORIENTED_EDGE('',*,*,#2088,.F.);
#2738=ORIENTED_EDGE('',*,*,#2073,.F.);
#2739=ORIENTED_EDGE('',*,*,#2077,.F.);
#2740=ORIENTED_EDGE('',*,*,#2080,.F.);
#2741=ORIENTED_EDGE('',*,*,#2083,.F.);
#2742=ORIENTED_EDGE('',*,*,#2086,.F.);
#2743=ORIENTED_EDGE('',*,*,#2089,.F.);
#2744=ORIENTED_EDGE('',*,*,#2090,.T.);
#2745=ORIENTED_EDGE('',*,*,#2091,.T.);
#2746=ORIENTED_EDGE('',*,*,#2092,.T.);
#2747=ORIENTED_EDGE('',*,*,#2093,.F.);
#2748=ORIENTED_EDGE('',*,*,#2092,.F.);
#2749=ORIENTED_EDGE('',*,*,#2094,.F.);
#2750=ORIENTED_EDGE('',*,*,#2095,.F.);
#2751=ORIENTED_EDGE('',*,*,#2096,.T.);
#2752=ORIENTED_EDGE('',*,*,#2097,.T.);
#2753=ORIENTED_EDGE('',*,*,#2094,.T.);
#2754=ORIENTED_EDGE('',*,*,#2091,.F.);
#2755=ORIENTED_EDGE('',*,*,#2098,.F.);
#2756=ORIENTED_EDGE('',*,*,#2095,.T.);
#2757=ORIENTED_EDGE('',*,*,#2097,.F.);
#2758=ORIENTED_EDGE('',*,*,#2099,.T.);
#2759=ORIENTED_EDGE('',*,*,#2100,.F.);
#2760=ORIENTED_EDGE('',*,*,#2099,.F.);
#2761=ORIENTED_EDGE('',*,*,#2096,.F.);
#2762=ORIENTED_EDGE('',*,*,#2090,.F.);
#2763=ORIENTED_EDGE('',*,*,#2101,.F.);
#2764=ORIENTED_EDGE('',*,*,#2102,.T.);
#2765=ORIENTED_EDGE('',*,*,#2103,.T.);
#2766=ORIENTED_EDGE('',*,*,#2102,.F.);
#2767=ORIENTED_EDGE('',*,*,#2098,.T.);
#2768=ORIENTED_EDGE('',*,*,#2100,.T.);
#2769=ORIENTED_EDGE('',*,*,#2089,.T.);
#2770=ORIENTED_EDGE('',*,*,#2093,.T.);
#2771=ORIENTED_EDGE('',*,*,#2101,.T.);
#2772=ORIENTED_EDGE('',*,*,#2103,.F.);
#2773=ORIENTED_EDGE('',*,*,#2104,.F.);
#2774=ORIENTED_EDGE('',*,*,#2105,.F.);
#2775=ORIENTED_EDGE('',*,*,#2106,.T.);
#2776=ORIENTED_EDGE('',*,*,#2104,.T.);
#2777=ORIENTED_EDGE('',*,*,#2106,.F.);
#2778=ORIENTED_EDGE('',*,*,#2107,.F.);
#2779=ORIENTED_EDGE('',*,*,#2108,.T.);
#2780=ORIENTED_EDGE('',*,*,#2105,.T.);
#2781=ORIENTED_EDGE('',*,*,#2108,.F.);
#2782=ORIENTED_EDGE('',*,*,#2107,.T.);
#2783=ORIENTED_EDGE('',*,*,#2109,.F.);
#2784=ORIENTED_EDGE('',*,*,#2110,.F.);
#2785=ORIENTED_EDGE('',*,*,#2111,.T.);
#2786=ORIENTED_EDGE('',*,*,#2109,.T.);
#2787=ORIENTED_EDGE('',*,*,#2111,.F.);
#2788=ORIENTED_EDGE('',*,*,#2110,.T.);
#2789=ORIENTED_EDGE('',*,*,#2112,.F.);
#2790=ORIENTED_EDGE('',*,*,#2113,.F.);
#2791=ORIENTED_EDGE('',*,*,#2114,.T.);
#2792=ORIENTED_EDGE('',*,*,#2115,.F.);
#2793=ORIENTED_EDGE('',*,*,#2116,.F.);
#2794=ORIENTED_EDGE('',*,*,#2114,.F.);
#2795=ORIENTED_EDGE('',*,*,#2117,.F.);
#2796=ORIENTED_EDGE('',*,*,#2118,.F.);
#2797=ORIENTED_EDGE('',*,*,#2119,.T.);
#2798=ORIENTED_EDGE('',*,*,#2120,.F.);
#2799=ORIENTED_EDGE('',*,*,#2121,.F.);
#2800=ORIENTED_EDGE('',*,*,#2122,.F.);
#2801=ORIENTED_EDGE('',*,*,#2123,.F.);
#2802=ORIENTED_EDGE('',*,*,#2119,.F.);
#2803=ORIENTED_EDGE('',*,*,#2124,.F.);
#2804=ORIENTED_EDGE('',*,*,#2125,.T.);
#2805=ORIENTED_EDGE('',*,*,#2126,.F.);
#2806=ORIENTED_EDGE('',*,*,#2127,.F.);
#2807=ORIENTED_EDGE('',*,*,#2128,.F.);
#2808=ORIENTED_EDGE('',*,*,#2129,.F.);
#2809=ORIENTED_EDGE('',*,*,#2130,.F.);
#2810=ORIENTED_EDGE('',*,*,#2131,.T.);
#2811=ORIENTED_EDGE('',*,*,#2132,.F.);
#2812=ORIENTED_EDGE('',*,*,#2131,.F.);
#2813=ORIENTED_EDGE('',*,*,#2133,.F.);
#2814=ORIENTED_EDGE('',*,*,#2125,.F.);
#2815=ORIENTED_EDGE('',*,*,#2134,.T.);
#2816=ORIENTED_EDGE('',*,*,#2126,.T.);
#2817=ORIENTED_EDGE('',*,*,#2133,.T.);
#2818=ORIENTED_EDGE('',*,*,#2130,.T.);
#2819=ORIENTED_EDGE('',*,*,#2135,.F.);
#2820=ORIENTED_EDGE('',*,*,#2127,.T.);
#2821=ORIENTED_EDGE('',*,*,#2135,.T.);
#2822=ORIENTED_EDGE('',*,*,#2129,.T.);
#2823=ORIENTED_EDGE('',*,*,#2136,.F.);
#2824=ORIENTED_EDGE('',*,*,#2117,.T.);
#2825=ORIENTED_EDGE('',*,*,#2118,.T.);
#2826=ORIENTED_EDGE('',*,*,#2137,.F.);
#2827=ORIENTED_EDGE('',*,*,#2138,.F.);
#2828=ORIENTED_EDGE('',*,*,#2139,.T.);
#2829=ORIENTED_EDGE('',*,*,#2140,.F.);
#2830=ORIENTED_EDGE('',*,*,#2139,.F.);
#2831=ORIENTED_EDGE('',*,*,#2141,.F.);
#2832=ORIENTED_EDGE('',*,*,#2142,.F.);
#2833=ORIENTED_EDGE('',*,*,#2143,.F.);
#2834=ORIENTED_EDGE('',*,*,#2144,.T.);
#2835=ORIENTED_EDGE('',*,*,#2145,.F.);
#2836=ORIENTED_EDGE('',*,*,#2144,.F.);
#2837=ORIENTED_EDGE('',*,*,#2146,.F.);
#2838=ORIENTED_EDGE('',*,*,#2147,.F.);
#2839=ORIENTED_EDGE('',*,*,#2148,.F.);
#2840=ORIENTED_EDGE('',*,*,#2149,.T.);
#2841=ORIENTED_EDGE('',*,*,#2150,.F.);
#2842=ORIENTED_EDGE('',*,*,#2149,.F.);
#2843=ORIENTED_EDGE('',*,*,#2151,.F.);
#2844=ORIENTED_EDGE('',*,*,#2152,.F.);
#2845=ORIENTED_EDGE('',*,*,#2124,.T.);
#2846=ORIENTED_EDGE('',*,*,#2136,.T.);
#2847=ORIENTED_EDGE('',*,*,#2128,.T.);
#2848=ORIENTED_EDGE('',*,*,#2132,.T.);
#2849=ORIENTED_EDGE('',*,*,#2134,.F.);
#2850=ORIENTED_EDGE('',*,*,#2153,.T.);
#2851=ORIENTED_EDGE('',*,*,#2122,.T.);
#2852=ORIENTED_EDGE('',*,*,#2121,.T.);
#2853=ORIENTED_EDGE('',*,*,#2154,.T.);
#2854=ORIENTED_EDGE('',*,*,#2152,.T.);
#2855=ORIENTED_EDGE('',*,*,#2154,.F.);
#2856=ORIENTED_EDGE('',*,*,#2120,.T.);
#2857=ORIENTED_EDGE('',*,*,#2123,.T.);
#2858=ORIENTED_EDGE('',*,*,#2153,.F.);
#2859=ORIENTED_EDGE('',*,*,#2140,.T.);
#2860=ORIENTED_EDGE('',*,*,#2145,.T.);
#2861=ORIENTED_EDGE('',*,*,#2150,.T.);
#2862=ORIENTED_EDGE('',*,*,#2155,.T.);
#2863=ORIENTED_EDGE('',*,*,#2156,.F.);
#2864=ORIENTED_EDGE('',*,*,#2141,.T.);
#2865=ORIENTED_EDGE('',*,*,#2157,.F.);
#2866=ORIENTED_EDGE('',*,*,#2146,.T.);
#2867=ORIENTED_EDGE('',*,*,#2158,.F.);
#2868=ORIENTED_EDGE('',*,*,#2151,.T.);
#2869=ORIENTED_EDGE('',*,*,#2159,.F.);
#2870=ORIENTED_EDGE('',*,*,#2155,.F.);
#2871=ORIENTED_EDGE('',*,*,#2159,.T.);
#2872=ORIENTED_EDGE('',*,*,#2148,.T.);
#2873=ORIENTED_EDGE('',*,*,#2147,.T.);
#2874=ORIENTED_EDGE('',*,*,#2158,.T.);
#2875=ORIENTED_EDGE('',*,*,#2143,.T.);
#2876=ORIENTED_EDGE('',*,*,#2142,.T.);
#2877=ORIENTED_EDGE('',*,*,#2157,.T.);
#2878=ORIENTED_EDGE('',*,*,#2138,.T.);
#2879=ORIENTED_EDGE('',*,*,#2137,.T.);
#2880=ORIENTED_EDGE('',*,*,#2156,.T.);
#2881=ORIENTED_EDGE('',*,*,#2112,.T.);
#2882=ORIENTED_EDGE('',*,*,#2113,.T.);
#2883=ORIENTED_EDGE('',*,*,#2115,.T.);
#2884=ORIENTED_EDGE('',*,*,#2116,.T.);
#2885=ORIENTED_EDGE('',*,*,#2160,.T.);
#2886=ORIENTED_EDGE('',*,*,#2161,.T.);
#2887=ORIENTED_EDGE('',*,*,#2162,.T.);
#2888=ORIENTED_EDGE('',*,*,#2163,.T.);
#2889=ORIENTED_EDGE('',*,*,#2164,.T.);
#2890=ORIENTED_EDGE('',*,*,#2165,.T.);
#2891=ORIENTED_EDGE('',*,*,#2160,.F.);
#2892=ORIENTED_EDGE('',*,*,#2166,.T.);
#2893=ORIENTED_EDGE('',*,*,#2167,.T.);
#2894=ORIENTED_EDGE('',*,*,#2168,.T.);
#2895=ORIENTED_EDGE('',*,*,#2164,.F.);
#2896=ORIENTED_EDGE('',*,*,#2169,.T.);
#2897=ORIENTED_EDGE('',*,*,#2162,.F.);
#2898=ORIENTED_EDGE('',*,*,#2170,.T.);
#2899=ORIENTED_EDGE('',*,*,#2167,.F.);
#2900=ORIENTED_EDGE('',*,*,#2171,.T.);
#2901=ORIENTED_EDGE('',*,*,#2166,.F.);
#2902=ORIENTED_EDGE('',*,*,#2172,.F.);
#2903=ORIENTED_EDGE('',*,*,#2173,.F.);
#2904=ORIENTED_EDGE('',*,*,#2174,.T.);
#2905=ORIENTED_EDGE('',*,*,#2163,.F.);
#2906=ORIENTED_EDGE('',*,*,#2175,.F.);
#2907=ORIENTED_EDGE('',*,*,#2176,.F.);
#2908=ORIENTED_EDGE('',*,*,#2172,.T.);
#2909=ORIENTED_EDGE('',*,*,#2161,.F.);
#2910=ORIENTED_EDGE('',*,*,#2165,.F.);
#2911=ORIENTED_EDGE('',*,*,#2168,.F.);
#2912=ORIENTED_EDGE('',*,*,#2170,.F.);
#2913=ORIENTED_EDGE('',*,*,#2177,.T.);
#2914=ORIENTED_EDGE('',*,*,#2176,.T.);
#2915=ORIENTED_EDGE('',*,*,#2178,.T.);
#2916=ORIENTED_EDGE('',*,*,#2179,.T.);
#2917=ORIENTED_EDGE('',*,*,#2180,.T.);
#2918=ORIENTED_EDGE('',*,*,#2173,.T.);
#2919=ORIENTED_EDGE('',*,*,#2177,.F.);
#2920=ORIENTED_EDGE('',*,*,#2181,.T.);
#2921=ORIENTED_EDGE('',*,*,#2182,.T.);
#2922=ORIENTED_EDGE('',*,*,#2183,.T.);
#2923=ORIENTED_EDGE('',*,*,#2180,.F.);
#2924=ORIENTED_EDGE('',*,*,#2184,.T.);
#2925=ORIENTED_EDGE('',*,*,#2178,.F.);
#2926=ORIENTED_EDGE('',*,*,#2185,.T.);
#2927=ORIENTED_EDGE('',*,*,#2182,.F.);
#2928=ORIENTED_EDGE('',*,*,#2186,.T.);
#2929=ORIENTED_EDGE('',*,*,#2171,.F.);
#2930=ORIENTED_EDGE('',*,*,#2187,.F.);
#2931=ORIENTED_EDGE('',*,*,#2185,.F.);
#2932=ORIENTED_EDGE('',*,*,#2175,.T.);
#2933=ORIENTED_EDGE('',*,*,#2179,.F.);
#2934=ORIENTED_EDGE('',*,*,#2186,.F.);
#2935=ORIENTED_EDGE('',*,*,#2184,.F.);
#2936=ORIENTED_EDGE('',*,*,#2181,.F.);
#2937=ORIENTED_EDGE('',*,*,#2169,.F.);
#2938=ORIENTED_EDGE('',*,*,#2174,.F.);
#2939=ORIENTED_EDGE('',*,*,#2183,.F.);
#2940=ORIENTED_EDGE('',*,*,#2187,.T.);
#2941=ORIENTED_EDGE('',*,*,#2188,.F.);
#2942=ORIENTED_EDGE('',*,*,#2189,.T.);
#2943=ORIENTED_EDGE('',*,*,#2190,.T.);
#2944=ORIENTED_EDGE('',*,*,#2191,.F.);
#2945=ORIENTED_EDGE('',*,*,#2192,.F.);
#2946=ORIENTED_EDGE('',*,*,#2193,.T.);
#2947=ORIENTED_EDGE('',*,*,#2194,.T.);
#2948=ORIENTED_EDGE('',*,*,#2189,.F.);
#2949=ORIENTED_EDGE('',*,*,#2195,.F.);
#2950=ORIENTED_EDGE('',*,*,#2196,.T.);
#2951=ORIENTED_EDGE('',*,*,#2197,.T.);
#2952=ORIENTED_EDGE('',*,*,#2193,.F.);
#2953=ORIENTED_EDGE('',*,*,#2198,.F.);
#2954=ORIENTED_EDGE('',*,*,#2199,.T.);
#2955=ORIENTED_EDGE('',*,*,#2200,.T.);
#2956=ORIENTED_EDGE('',*,*,#2196,.F.);
#2957=ORIENTED_EDGE('',*,*,#2201,.F.);
#2958=ORIENTED_EDGE('',*,*,#2202,.T.);
#2959=ORIENTED_EDGE('',*,*,#2203,.T.);
#2960=ORIENTED_EDGE('',*,*,#2199,.F.);
#2961=ORIENTED_EDGE('',*,*,#2204,.F.);
#2962=ORIENTED_EDGE('',*,*,#2191,.T.);
#2963=ORIENTED_EDGE('',*,*,#2205,.T.);
#2964=ORIENTED_EDGE('',*,*,#2202,.F.);
#2965=ORIENTED_EDGE('',*,*,#2205,.F.);
#2966=ORIENTED_EDGE('',*,*,#2190,.F.);
#2967=ORIENTED_EDGE('',*,*,#2194,.F.);
#2968=ORIENTED_EDGE('',*,*,#2197,.F.);
#2969=ORIENTED_EDGE('',*,*,#2200,.F.);
#2970=ORIENTED_EDGE('',*,*,#2203,.F.);
#2971=ORIENTED_EDGE('',*,*,#2206,.F.);
#2972=ORIENTED_EDGE('',*,*,#2188,.T.);
#2973=ORIENTED_EDGE('',*,*,#2204,.T.);
#2974=ORIENTED_EDGE('',*,*,#2201,.T.);
#2975=ORIENTED_EDGE('',*,*,#2198,.T.);
#2976=ORIENTED_EDGE('',*,*,#2195,.T.);
#2977=ORIENTED_EDGE('',*,*,#2192,.T.);
#2978=ORIENTED_EDGE('',*,*,#2207,.F.);
#2979=ORIENTED_EDGE('',*,*,#2208,.T.);
#2980=ORIENTED_EDGE('',*,*,#2206,.T.);
#2981=ORIENTED_EDGE('',*,*,#2208,.F.);
#2982=ORIENTED_EDGE('',*,*,#2209,.F.);
#2983=ORIENTED_EDGE('',*,*,#2210,.T.);
#2984=ORIENTED_EDGE('',*,*,#2207,.T.);
#2985=ORIENTED_EDGE('',*,*,#2210,.F.);
#2986=ORIENTED_EDGE('',*,*,#2211,.F.);
#2987=ORIENTED_EDGE('',*,*,#2212,.T.);
#2988=ORIENTED_EDGE('',*,*,#2209,.T.);
#2989=ORIENTED_EDGE('',*,*,#2212,.F.);
#2990=ORIENTED_EDGE('',*,*,#2211,.T.);
#2991=ORIENTED_EDGE('',*,*,#2213,.F.);
#2992=ORIENTED_EDGE('',*,*,#2214,.T.);
#2993=ORIENTED_EDGE('',*,*,#2215,.F.);
#2994=ORIENTED_EDGE('',*,*,#2214,.F.);
#2995=ORIENTED_EDGE('',*,*,#2216,.F.);
#2996=ORIENTED_EDGE('',*,*,#2217,.T.);
#2997=ORIENTED_EDGE('',*,*,#2218,.F.);
#2998=ORIENTED_EDGE('',*,*,#2219,.T.);
#2999=ORIENTED_EDGE('',*,*,#2216,.T.);
#3000=ORIENTED_EDGE('',*,*,#2219,.F.);
#3001=ORIENTED_EDGE('',*,*,#2220,.F.);
#3002=ORIENTED_EDGE('',*,*,#2221,.T.);
#3003=ORIENTED_EDGE('',*,*,#2218,.T.);
#3004=ORIENTED_EDGE('',*,*,#2221,.F.);
#3005=ORIENTED_EDGE('',*,*,#2215,.T.);
#3006=ORIENTED_EDGE('',*,*,#2222,.F.);
#3007=ORIENTED_EDGE('',*,*,#2223,.T.);
#3008=ORIENTED_EDGE('',*,*,#2220,.T.);
#3009=ORIENTED_EDGE('',*,*,#2223,.F.);
#3010=ORIENTED_EDGE('',*,*,#2222,.T.);
#3011=ORIENTED_EDGE('',*,*,#2224,.F.);
#3012=ORIENTED_EDGE('',*,*,#2224,.T.);
#3013=ORIENTED_EDGE('',*,*,#2225,.T.);
#3014=ORIENTED_EDGE('',*,*,#2217,.F.);
#3015=ORIENTED_EDGE('',*,*,#2225,.F.);
#3016=ORIENTED_EDGE('',*,*,#2213,.T.);
#3017=ORIENTED_EDGE('',*,*,#2226,.F.);
#3018=ORIENTED_EDGE('',*,*,#2227,.T.);
#3019=ORIENTED_EDGE('',*,*,#2228,.T.);
#3020=ORIENTED_EDGE('',*,*,#2229,.F.);
#3021=ORIENTED_EDGE('',*,*,#2230,.F.);
#3022=ORIENTED_EDGE('',*,*,#2231,.T.);
#3023=ORIENTED_EDGE('',*,*,#2232,.T.);
#3024=ORIENTED_EDGE('',*,*,#2227,.F.);
#3025=ORIENTED_EDGE('',*,*,#2233,.F.);
#3026=ORIENTED_EDGE('',*,*,#2234,.T.);
#3027=ORIENTED_EDGE('',*,*,#2235,.T.);
#3028=ORIENTED_EDGE('',*,*,#2231,.F.);
#3029=ORIENTED_EDGE('',*,*,#2236,.F.);
#3030=ORIENTED_EDGE('',*,*,#2237,.T.);
#3031=ORIENTED_EDGE('',*,*,#2238,.T.);
#3032=ORIENTED_EDGE('',*,*,#2234,.F.);
#3033=ORIENTED_EDGE('',*,*,#2239,.F.);
#3034=ORIENTED_EDGE('',*,*,#2240,.T.);
#3035=ORIENTED_EDGE('',*,*,#2241,.T.);
#3036=ORIENTED_EDGE('',*,*,#2237,.F.);
#3037=ORIENTED_EDGE('',*,*,#2242,.F.);
#3038=ORIENTED_EDGE('',*,*,#2229,.T.);
#3039=ORIENTED_EDGE('',*,*,#2243,.T.);
#3040=ORIENTED_EDGE('',*,*,#2240,.F.);
#3041=ORIENTED_EDGE('',*,*,#2243,.F.);
#3042=ORIENTED_EDGE('',*,*,#2228,.F.);
#3043=ORIENTED_EDGE('',*,*,#2232,.F.);
#3044=ORIENTED_EDGE('',*,*,#2235,.F.);
#3045=ORIENTED_EDGE('',*,*,#2238,.F.);
#3046=ORIENTED_EDGE('',*,*,#2241,.F.);
#3047=ORIENTED_EDGE('',*,*,#2244,.F.);
#3048=ORIENTED_EDGE('',*,*,#2226,.T.);
#3049=ORIENTED_EDGE('',*,*,#2242,.T.);
#3050=ORIENTED_EDGE('',*,*,#2239,.T.);
#3051=ORIENTED_EDGE('',*,*,#2236,.T.);
#3052=ORIENTED_EDGE('',*,*,#2233,.T.);
#3053=ORIENTED_EDGE('',*,*,#2230,.T.);
#3054=ORIENTED_EDGE('',*,*,#2245,.F.);
#3055=ORIENTED_EDGE('',*,*,#2246,.T.);
#3056=ORIENTED_EDGE('',*,*,#2244,.T.);
#3057=ORIENTED_EDGE('',*,*,#2246,.F.);
#3058=ORIENTED_EDGE('',*,*,#2247,.F.);
#3059=ORIENTED_EDGE('',*,*,#2248,.T.);
#3060=ORIENTED_EDGE('',*,*,#2245,.T.);
#3061=ORIENTED_EDGE('',*,*,#2248,.F.);
#3062=ORIENTED_EDGE('',*,*,#2249,.F.);
#3063=ORIENTED_EDGE('',*,*,#2250,.T.);
#3064=ORIENTED_EDGE('',*,*,#2247,.T.);
#3065=ORIENTED_EDGE('',*,*,#2250,.F.);
#3066=ORIENTED_EDGE('',*,*,#2249,.T.);
#3067=CYLINDRICAL_SURFACE('',#3555,0.34);
#3068=CYLINDRICAL_SURFACE('',#3558,0.34);
#3069=CYLINDRICAL_SURFACE('',#3561,0.34);
#3070=CYLINDRICAL_SURFACE('',#3564,0.34);
#3071=CYLINDRICAL_SURFACE('',#3567,3.01);
#3072=CYLINDRICAL_SURFACE('',#3575,0.34);
#3073=CYLINDRICAL_SURFACE('',#3578,0.34);
#3074=CYLINDRICAL_SURFACE('',#3581,0.34);
#3075=CYLINDRICAL_SURFACE('',#3584,0.34);
#3076=CYLINDRICAL_SURFACE('',#3587,3.01);
#3077=CYLINDRICAL_SURFACE('',#3602,0.425);
#3078=CYLINDRICAL_SURFACE('',#3605,0.595);
#3079=CYLINDRICAL_SURFACE('',#3611,0.425);
#3080=CYLINDRICAL_SURFACE('',#3614,0.595);
#3081=CYLINDRICAL_SURFACE('',#3620,0.425);
#3082=CYLINDRICAL_SURFACE('',#3623,0.595);
#3083=CYLINDRICAL_SURFACE('',#3629,0.425);
#3084=CYLINDRICAL_SURFACE('',#3632,0.595);
#3085=CYLINDRICAL_SURFACE('',#3638,0.425);
#3086=CYLINDRICAL_SURFACE('',#3641,0.595);
#3087=CYLINDRICAL_SURFACE('',#3647,0.425);
#3088=CYLINDRICAL_SURFACE('',#3650,0.595);
#3089=CYLINDRICAL_SURFACE('',#3656,0.425);
#3090=CYLINDRICAL_SURFACE('',#3659,0.595);
#3091=CYLINDRICAL_SURFACE('',#3665,0.425);
#3092=CYLINDRICAL_SURFACE('',#3668,0.595);
#3093=CYLINDRICAL_SURFACE('',#3675,2.05);
#3094=CYLINDRICAL_SURFACE('',#3678,2.05);
#3095=CYLINDRICAL_SURFACE('',#3683,3.);
#3096=CYLINDRICAL_SURFACE('',#3686,3.);
#3097=CYLINDRICAL_SURFACE('',#3691,0.6);
#3098=CYLINDRICAL_SURFACE('',#3694,0.6);
#3099=CYLINDRICAL_SURFACE('',#3697,0.6);
#3100=CYLINDRICAL_SURFACE('',#3700,0.6);
#3101=CYLINDRICAL_SURFACE('',#3714,1.8);
#3102=CYLINDRICAL_SURFACE('',#3723,0.25);
#3103=CYLINDRICAL_SURFACE('',#3724,0.25);
#3104=CYLINDRICAL_SURFACE('',#3725,1.65);
#3105=CYLINDRICAL_SURFACE('',#3728,0.25);
#3106=CYLINDRICAL_SURFACE('',#3729,0.25);
#3107=CYLINDRICAL_SURFACE('',#3730,0.25);
#3108=CYLINDRICAL_SURFACE('',#3731,0.25);
#3109=CYLINDRICAL_SURFACE('',#3736,1.75);
#3110=CYLINDRICAL_SURFACE('',#3740,0.6);
#3111=CYLINDRICAL_SURFACE('',#3744,0.42);
#3112=CYLINDRICAL_SURFACE('',#3747,0.8);
#3113=CYLINDRICAL_SURFACE('',#3757,0.65);
#3114=CYLINDRICAL_SURFACE('',#3765,0.3933);
#3115=CYLINDRICAL_SURFACE('',#3814,0.6);
#3116=CYLINDRICAL_SURFACE('',#3825,0.8);
#3117=CYLINDRICAL_SURFACE('',#3829,0.399999999999999);
#3118=CYLINDRICAL_SURFACE('',#3832,0.4);
#3119=CYLINDRICAL_SURFACE('',#3833,0.25175);
#3120=CYLINDRICAL_SURFACE('',#3840,0.6);
#3121=CYLINDRICAL_SURFACE('',#3842,0.4);
#3122=CYLINDRICAL_SURFACE('',#3843,0.4);
#3123=CYLINDRICAL_SURFACE('',#3844,0.4);
#3124=CYLINDRICAL_SURFACE('',#3847,1.6);
#3125=CYLINDRICAL_SURFACE('',#3864,0.2);
#3126=CYLINDRICAL_SURFACE('',#3875,0.2);
#3127=CYLINDRICAL_SURFACE('',#3890,0.2942);
#3128=CYLINDRICAL_SURFACE('',#3896,0.2117);
#3129=CYLINDRICAL_SURFACE('',#3902,1.1);
#3130=CYLINDRICAL_SURFACE('',#3908,0.6);
#3131=CYLINDRICAL_SURFACE('',#3921,0.24505);
#3132=ADVANCED_FACE('',(#515),#3067,.F.);
#3133=ADVANCED_FACE('',(#516),#3068,.F.);
#3134=ADVANCED_FACE('',(#517),#3069,.F.);
#3135=ADVANCED_FACE('',(#518),#3070,.F.);
#3136=ADVANCED_FACE('',(#519),#3071,.F.);
#3137=ADVANCED_FACE('',(#520),#410,.T.);
#3138=ADVANCED_FACE('',(#521),#411,.T.);
#3139=ADVANCED_FACE('',(#522),#412,.T.);
#3140=ADVANCED_FACE('',(#523,#320,#321,#322,#323,#324),#413,.T.);
#3141=ADVANCED_FACE('',(#524,#325,#326,#327,#328,#329),#414,.F.);
#3142=ADVANCED_FACE('',(#525),#3072,.F.);
#3143=ADVANCED_FACE('',(#526),#3073,.F.);
#3144=ADVANCED_FACE('',(#527),#3074,.F.);
#3145=ADVANCED_FACE('',(#528),#3075,.F.);
#3146=ADVANCED_FACE('',(#529),#3076,.F.);
#3147=ADVANCED_FACE('',(#530),#415,.T.);
#3148=ADVANCED_FACE('',(#531),#416,.T.);
#3149=ADVANCED_FACE('',(#532),#417,.T.);
#3150=ADVANCED_FACE('',(#533,#330,#331,#332,#333,#334),#418,.T.);
#3151=ADVANCED_FACE('',(#534,#335,#336,#337,#338,#339),#419,.F.);
#3152=ADVANCED_FACE('',(#535),#420,.T.);
#3153=ADVANCED_FACE('',(#536),#421,.T.);
#3154=ADVANCED_FACE('',(#537),#422,.T.);
#3155=ADVANCED_FACE('',(#538),#423,.T.);
#3156=ADVANCED_FACE('',(#539,#340,#341),#424,.T.);
#3157=ADVANCED_FACE('',(#540),#425,.F.);
#3158=ADVANCED_FACE('',(#541),#3077,.F.);
#3159=ADVANCED_FACE('',(#542),#3078,.T.);
#3160=ADVANCED_FACE('',(#543,#342),#426,.T.);
#3161=ADVANCED_FACE('',(#544,#343),#427,.F.);
#3162=ADVANCED_FACE('',(#545),#3079,.F.);
#3163=ADVANCED_FACE('',(#546),#3080,.T.);
#3164=ADVANCED_FACE('',(#547,#344),#428,.T.);
#3165=ADVANCED_FACE('',(#548,#345),#429,.F.);
#3166=ADVANCED_FACE('',(#549),#3081,.F.);
#3167=ADVANCED_FACE('',(#550),#3082,.T.);
#3168=ADVANCED_FACE('',(#551,#346),#430,.T.);
#3169=ADVANCED_FACE('',(#552,#347),#431,.F.);
#3170=ADVANCED_FACE('',(#553),#3083,.F.);
#3171=ADVANCED_FACE('',(#554),#3084,.T.);
#3172=ADVANCED_FACE('',(#555,#348),#432,.T.);
#3173=ADVANCED_FACE('',(#556,#349),#433,.F.);
#3174=ADVANCED_FACE('',(#557),#3085,.F.);
#3175=ADVANCED_FACE('',(#558),#3086,.T.);
#3176=ADVANCED_FACE('',(#559,#350),#434,.T.);
#3177=ADVANCED_FACE('',(#560,#351),#435,.F.);
#3178=ADVANCED_FACE('',(#561),#3087,.F.);
#3179=ADVANCED_FACE('',(#562),#3088,.T.);
#3180=ADVANCED_FACE('',(#563,#352),#436,.T.);
#3181=ADVANCED_FACE('',(#564,#353),#437,.F.);
#3182=ADVANCED_FACE('',(#565),#3089,.F.);
#3183=ADVANCED_FACE('',(#566),#3090,.T.);
#3184=ADVANCED_FACE('',(#567,#354),#438,.T.);
#3185=ADVANCED_FACE('',(#568,#355),#439,.F.);
#3186=ADVANCED_FACE('',(#569),#3091,.F.);
#3187=ADVANCED_FACE('',(#570),#3092,.T.);
#3188=ADVANCED_FACE('',(#571,#356),#440,.T.);
#3189=ADVANCED_FACE('',(#572,#357),#441,.F.);
#3190=ADVANCED_FACE('',(#573),#3093,.F.);
#3191=ADVANCED_FACE('',(#574),#3094,.F.);
#3192=ADVANCED_FACE('',(#575,#358,#359),#237,.F.);
#3193=ADVANCED_FACE('',(#576),#3095,.T.);
#3194=ADVANCED_FACE('',(#577),#3096,.T.);
#3195=ADVANCED_FACE('',(#578,#360),#442,.F.);
#3196=ADVANCED_FACE('',(#579,#361),#443,.T.);
#3197=ADVANCED_FACE('',(#580),#3097,.F.);
#3198=ADVANCED_FACE('',(#581),#3098,.F.);
#3199=ADVANCED_FACE('',(#582),#3099,.F.);
#3200=ADVANCED_FACE('',(#583),#3100,.F.);
#3201=ADVANCED_FACE('',(#584),#444,.T.);
#3202=ADVANCED_FACE('',(#585),#445,.T.);
#3203=ADVANCED_FACE('',(#586),#446,.T.);
#3204=ADVANCED_FACE('',(#587),#447,.T.);
#3205=ADVANCED_FACE('',(#588),#448,.T.);
#3206=ADVANCED_FACE('',(#589),#449,.T.);
#3207=ADVANCED_FACE('',(#590),#450,.T.);
#3208=ADVANCED_FACE('',(#591),#451,.T.);
#3209=ADVANCED_FACE('',(#592,#362,#363,#364,#365,#366),#452,.T.);
#3210=ADVANCED_FACE('',(#593,#367,#368,#369,#370,#371),#453,.F.);
#3211=ADVANCED_FACE('',(#594),#3101,.F.);
#3212=ADVANCED_FACE('',(#595,#372),#454,.T.);
#3213=ADVANCED_FACE('',(#596,#373,#374),#238,.T.);
#3214=ADVANCED_FACE('',(#597,#375),#455,.T.);
#3215=ADVANCED_FACE('',(#598),#3102,.F.);
#3216=ADVANCED_FACE('',(#599),#3103,.F.);
#3217=ADVANCED_FACE('',(#600,#376,#377,#378,#379,#380,#381),#3104,.T.);
#3218=ADVANCED_FACE('',(#601),#3105,.F.);
#3219=ADVANCED_FACE('',(#602),#3106,.F.);
#3220=ADVANCED_FACE('',(#603),#3107,.F.);
#3221=ADVANCED_FACE('',(#604),#3108,.F.);
#3222=ADVANCED_FACE('',(#605,#382),#456,.T.);
#3223=ADVANCED_FACE('',(#606,#383),#457,.T.);
#3224=ADVANCED_FACE('',(#607),#3109,.T.);
#3225=ADVANCED_FACE('',(#608,#384),#458,.T.);
#3226=ADVANCED_FACE('',(#609,#385,#386,#387,#388,#389,#390),#3110,.F.);
#3227=ADVANCED_FACE('',(#610),#3111,.F.);
#3228=ADVANCED_FACE('',(#611),#3112,.T.);
#3229=ADVANCED_FACE('',(#612,#391),#459,.T.);
#3230=ADVANCED_FACE('',(#613,#392),#460,.F.);
#3231=ADVANCED_FACE('',(#614),#461,.T.);
#3232=ADVANCED_FACE('',(#615),#13,.T.);
#3233=ADVANCED_FACE('',(#616),#3113,.T.);
#3234=ADVANCED_FACE('',(#617),#14,.T.);
#3235=ADVANCED_FACE('',(#618,#393),#462,.T.);
#3236=ADVANCED_FACE('',(#619),#15,.T.);
#3237=ADVANCED_FACE('',(#620),#3114,.T.);
#3238=ADVANCED_FACE('',(#621),#16,.T.);
#3239=ADVANCED_FACE('',(#622),#463,.T.);
#3240=ADVANCED_FACE('',(#623),#464,.F.);
#3241=ADVANCED_FACE('',(#624),#465,.F.);
#3242=ADVANCED_FACE('',(#625),#466,.F.);
#3243=ADVANCED_FACE('',(#626),#467,.F.);
#3244=ADVANCED_FACE('',(#627),#468,.F.);
#3245=ADVANCED_FACE('',(#628),#469,.F.);
#3246=ADVANCED_FACE('',(#629),#470,.F.);
#3247=ADVANCED_FACE('',(#630),#471,.F.);
#3248=ADVANCED_FACE('',(#631),#472,.F.);
#3249=ADVANCED_FACE('',(#632),#473,.F.);
#3250=ADVANCED_FACE('',(#633),#474,.F.);
#3251=ADVANCED_FACE('',(#634),#475,.F.);
#3252=ADVANCED_FACE('',(#635),#476,.T.);
#3253=ADVANCED_FACE('',(#636,#394),#3115,.T.);
#3254=ADVANCED_FACE('',(#637),#477,.T.);
#3255=ADVANCED_FACE('',(#638),#478,.F.);
#3256=ADVANCED_FACE('',(#639),#479,.T.);
#3257=ADVANCED_FACE('',(#640),#17,.T.);
#3258=ADVANCED_FACE('',(#641),#3116,.T.);
#3259=ADVANCED_FACE('',(#642,#395),#480,.T.);
#3260=ADVANCED_FACE('',(#643),#3117,.T.);
#3261=ADVANCED_FACE('',(#644),#481,.T.);
#3262=ADVANCED_FACE('',(#645),#3118,.F.);
#3263=ADVANCED_FACE('',(#646),#3119,.F.);
#3264=ADVANCED_FACE('',(#647),#482,.F.);
#3265=ADVANCED_FACE('',(#648),#483,.F.);
#3266=ADVANCED_FACE('',(#649),#484,.F.);
#3267=ADVANCED_FACE('',(#650,#396),#485,.T.);
#3268=ADVANCED_FACE('',(#651,#397),#3120,.F.);
#3269=ADVANCED_FACE('',(#652),#3121,.T.);
#3270=ADVANCED_FACE('',(#653),#3122,.T.);
#3271=ADVANCED_FACE('',(#654),#3123,.T.);
#3272=ADVANCED_FACE('',(#655,#398),#486,.T.);
#3273=ADVANCED_FACE('',(#656,#399,#400,#401),#3124,.T.);
#3274=ADVANCED_FACE('',(#657,#402,#403),#11,.T.);
#3275=ADVANCED_FACE('',(#658),#487,.T.);
#3276=ADVANCED_FACE('',(#659),#18,.T.);
#3277=ADVANCED_FACE('',(#660),#488,.T.);
#3278=ADVANCED_FACE('',(#661),#19,.T.);
#3279=ADVANCED_FACE('',(#662),#3125,.T.);
#3280=ADVANCED_FACE('',(#663),#489,.T.);
#3281=ADVANCED_FACE('',(#664),#490,.T.);
#3282=ADVANCED_FACE('',(#665),#491,.T.);
#3283=ADVANCED_FACE('',(#666),#20,.T.);
#3284=ADVANCED_FACE('',(#667),#492,.T.);
#3285=ADVANCED_FACE('',(#668),#21,.T.);
#3286=ADVANCED_FACE('',(#669),#3126,.T.);
#3287=ADVANCED_FACE('',(#670),#493,.F.);
#3288=ADVANCED_FACE('',(#671),#494,.T.);
#3289=ADVANCED_FACE('',(#672),#495,.F.);
#3290=ADVANCED_FACE('',(#673),#496,.F.);
#3291=ADVANCED_FACE('',(#674),#497,.F.);
#3292=ADVANCED_FACE('',(#675),#498,.F.);
#3293=ADVANCED_FACE('',(#676),#499,.F.);
#3294=ADVANCED_FACE('',(#677),#500,.F.);
#3295=ADVANCED_FACE('',(#678),#501,.F.);
#3296=ADVANCED_FACE('',(#679,#404),#502,.T.);
#3297=ADVANCED_FACE('',(#680),#22,.T.);
#3298=ADVANCED_FACE('',(#681),#3127,.T.);
#3299=ADVANCED_FACE('',(#682),#23,.T.);
#3300=ADVANCED_FACE('',(#683),#503,.T.);
#3301=ADVANCED_FACE('',(#684),#3128,.F.);
#3302=ADVANCED_FACE('',(#685,#405),#504,.T.);
#3303=ADVANCED_FACE('',(#686),#24,.T.);
#3304=ADVANCED_FACE('',(#687,#406),#3129,.T.);
#3305=ADVANCED_FACE('',(#688),#25,.T.);
#3306=ADVANCED_FACE('',(#689,#407),#505,.T.);
#3307=ADVANCED_FACE('',(#690,#408),#3130,.F.);
#3308=ADVANCED_FACE('',(#691),#506,.F.);
#3309=ADVANCED_FACE('',(#692),#507,.F.);
#3310=ADVANCED_FACE('',(#693),#508,.F.);
#3311=ADVANCED_FACE('',(#694),#509,.F.);
#3312=ADVANCED_FACE('',(#695),#510,.F.);
#3313=ADVANCED_FACE('',(#696),#511,.F.);
#3314=ADVANCED_FACE('',(#697),#512,.F.);
#3315=ADVANCED_FACE('',(#698,#409),#513,.T.);
#3316=ADVANCED_FACE('',(#699),#26,.T.);
#3317=ADVANCED_FACE('',(#700),#3131,.T.);
#3318=ADVANCED_FACE('',(#701),#27,.T.);
#3319=ADVANCED_FACE('',(#702),#514,.T.);
#3320=CLOSED_SHELL('',(#3132,#3133,#3134,#3135,#3136,#3137,#3138,#3139,
#3140,#3141,#3142,#3143,#3144,#3145,#3146,#3147,#3148,#3149,#3150,#3151,
#3152,#3153,#3154,#3155,#3156,#3157));
#3321=CLOSED_SHELL('',(#3158,#3159,#3160,#3161));
#3322=CLOSED_SHELL('',(#3162,#3163,#3164,#3165));
#3323=CLOSED_SHELL('',(#3166,#3167,#3168,#3169));
#3324=CLOSED_SHELL('',(#3170,#3171,#3172,#3173));
#3325=CLOSED_SHELL('',(#3174,#3175,#3176,#3177));
#3326=CLOSED_SHELL('',(#3178,#3179,#3180,#3181));
#3327=CLOSED_SHELL('',(#3182,#3183,#3184,#3185));
#3328=CLOSED_SHELL('',(#3186,#3187,#3188,#3189));
#3329=CLOSED_SHELL('',(#3190,#3191,#3192,#3193,#3194,#3195,#3196,#3197,
#3198,#3199,#3200,#3201,#3202,#3203,#3204,#3205,#3206,#3207,#3208,#3209,
#3210));
#3330=CLOSED_SHELL('',(#3211,#3212,#3213,#3214));
#3331=CLOSED_SHELL('',(#3215,#3216,#3217,#3218,#3219,#3220,#3221,#3222,
#3223,#3224,#3225,#3226));
#3332=CLOSED_SHELL('',(#3227,#3228,#3229,#3230));
#3333=CLOSED_SHELL('',(#3231,#3232,#3233,#3234,#3235,#3236,#3237,#3238,
#3239));
#3334=CLOSED_SHELL('',(#3240,#3241,#3242,#3243,#3244,#3245,#3246,#3247));
#3335=CLOSED_SHELL('',(#3248,#3249,#3250,#3251,#3252,#3253,#3254,#3255));
#3336=CLOSED_SHELL('',(#3256,#3257,#3258,#3259,#3260,#3261));
#3337=CLOSED_SHELL('',(#3262,#3263,#3264,#3265,#3266,#3267,#3268,#3269,
#3270,#3271,#3272,#3273,#3274));
#3338=CLOSED_SHELL('',(#3275,#3276,#3277,#3278,#3279,#3280,#3281,#3282,
#3283,#3284,#3285,#3286,#3287,#3288));
#3339=CLOSED_SHELL('',(#3289,#3290,#3291,#3292,#3293,#3294,#3295,#3296,
#3297,#3298,#3299,#3300));
#3340=CLOSED_SHELL('',(#3301,#3302,#3303,#3304,#3305,#3306,#3307));
#3341=CLOSED_SHELL('',(#3308,#3309,#3310,#3311,#3312,#3313,#3314,#3315,
#3316,#3317,#3318,#3319));
#3342=DERIVED_UNIT_ELEMENT(#3380,1.);
#3343=DERIVED_UNIT_ELEMENT(#6807,-3.);
#3344=DERIVED_UNIT_ELEMENT(#3380,1.);
#3345=DERIVED_UNIT_ELEMENT(#6807,-3.);
#3346=DERIVED_UNIT_ELEMENT(#3380,1.);
#3347=DERIVED_UNIT_ELEMENT(#6807,-3.);
#3348=DERIVED_UNIT_ELEMENT(#3380,1.);
#3349=DERIVED_UNIT_ELEMENT(#6807,-3.);
#3350=DERIVED_UNIT_ELEMENT(#3380,1.);
#3351=DERIVED_UNIT_ELEMENT(#6807,-3.);
#3352=DERIVED_UNIT_ELEMENT(#3380,1.);
#3353=DERIVED_UNIT_ELEMENT(#6807,-3.);
#3354=DERIVED_UNIT_ELEMENT(#3380,1.);
#3355=DERIVED_UNIT_ELEMENT(#6807,-3.);
#3356=DERIVED_UNIT_ELEMENT(#3380,1.);
#3357=DERIVED_UNIT_ELEMENT(#6807,-3.);
#3358=DERIVED_UNIT_ELEMENT(#3380,1.);
#3359=DERIVED_UNIT_ELEMENT(#6807,-3.);
#3360=DERIVED_UNIT_ELEMENT(#3380,1.);
#3361=DERIVED_UNIT_ELEMENT(#6807,-3.);
#3362=DERIVED_UNIT_ELEMENT(#3380,1.);
#3363=DERIVED_UNIT_ELEMENT(#6807,-3.);
#3364=DERIVED_UNIT_ELEMENT(#3380,1.);
#3365=DERIVED_UNIT_ELEMENT(#6807,-3.);
#3366=DERIVED_UNIT_ELEMENT(#3380,1.);
#3367=DERIVED_UNIT_ELEMENT(#6807,-3.);
#3368=DERIVED_UNIT_ELEMENT(#3380,1.);
#3369=DERIVED_UNIT_ELEMENT(#6807,-3.);
#3370=DERIVED_UNIT_ELEMENT(#3380,1.);
#3371=DERIVED_UNIT_ELEMENT(#6807,-3.);
#3372=DERIVED_UNIT_ELEMENT(#3380,1.);
#3373=DERIVED_UNIT_ELEMENT(#6807,-3.);
#3374=DERIVED_UNIT_ELEMENT(#3380,1.);
#3375=DERIVED_UNIT_ELEMENT(#6807,-3.);
#3376=DERIVED_UNIT_ELEMENT(#3380,1.);
#3377=DERIVED_UNIT_ELEMENT(#6807,-3.);
#3378=DERIVED_UNIT_ELEMENT(#3380,1.);
#3379=DERIVED_UNIT_ELEMENT(#6807,-3.);
#3380=(
MASS_UNIT()
NAMED_UNIT(*)
SI_UNIT(.KILO.,.GRAM.)
);
#3381=DERIVED_UNIT((#3342,#3343));
#3382=DERIVED_UNIT((#3344,#3345));
#3383=DERIVED_UNIT((#3346,#3347));
#3384=DERIVED_UNIT((#3348,#3349));
#3385=DERIVED_UNIT((#3350,#3351));
#3386=DERIVED_UNIT((#3352,#3353));
#3387=DERIVED_UNIT((#3354,#3355));
#3388=DERIVED_UNIT((#3356,#3357));
#3389=DERIVED_UNIT((#3358,#3359));
#3390=DERIVED_UNIT((#3360,#3361));
#3391=DERIVED_UNIT((#3362,#3363));
#3392=DERIVED_UNIT((#3364,#3365));
#3393=DERIVED_UNIT((#3366,#3367));
#3394=DERIVED_UNIT((#3368,#3369));
#3395=DERIVED_UNIT((#3370,#3371));
#3396=DERIVED_UNIT((#3372,#3373));
#3397=DERIVED_UNIT((#3374,#3375));
#3398=DERIVED_UNIT((#3376,#3377));
#3399=DERIVED_UNIT((#3378,#3379));
#3400=MEASURE_REPRESENTATION_ITEM('density measure',
POSITIVE_RATIO_MEASURE(7850.),#3381);
#3401=MEASURE_REPRESENTATION_ITEM('density measure',
POSITIVE_RATIO_MEASURE(7850.),#3382);
#3402=MEASURE_REPRESENTATION_ITEM('density measure',
POSITIVE_RATIO_MEASURE(7850.),#3383);
#3403=MEASURE_REPRESENTATION_ITEM('density measure',
POSITIVE_RATIO_MEASURE(7850.),#3384);
#3404=MEASURE_REPRESENTATION_ITEM('density measure',
POSITIVE_RATIO_MEASURE(7850.),#3385);
#3405=MEASURE_REPRESENTATION_ITEM('density measure',
POSITIVE_RATIO_MEASURE(7850.),#3386);
#3406=MEASURE_REPRESENTATION_ITEM('density measure',
POSITIVE_RATIO_MEASURE(7850.),#3387);
#3407=MEASURE_REPRESENTATION_ITEM('density measure',
POSITIVE_RATIO_MEASURE(7850.),#3388);
#3408=MEASURE_REPRESENTATION_ITEM('density measure',
POSITIVE_RATIO_MEASURE(7850.),#3389);
#3409=MEASURE_REPRESENTATION_ITEM('density measure',
POSITIVE_RATIO_MEASURE(7850.),#3390);
#3410=MEASURE_REPRESENTATION_ITEM('density measure',
POSITIVE_RATIO_MEASURE(7850.),#3391);
#3411=MEASURE_REPRESENTATION_ITEM('density measure',
POSITIVE_RATIO_MEASURE(7850.),#3392);
#3412=MEASURE_REPRESENTATION_ITEM('density measure',
POSITIVE_RATIO_MEASURE(7850.),#3393);
#3413=MEASURE_REPRESENTATION_ITEM('density measure',
POSITIVE_RATIO_MEASURE(7850.),#3394);
#3414=MEASURE_REPRESENTATION_ITEM('density measure',
POSITIVE_RATIO_MEASURE(7850.),#3395);
#3415=MEASURE_REPRESENTATION_ITEM('density measure',
POSITIVE_RATIO_MEASURE(7850.),#3396);
#3416=MEASURE_REPRESENTATION_ITEM('density measure',
POSITIVE_RATIO_MEASURE(7850.),#3397);
#3417=MEASURE_REPRESENTATION_ITEM('density measure',
POSITIVE_RATIO_MEASURE(7850.),#3398);
#3418=MEASURE_REPRESENTATION_ITEM('density measure',
POSITIVE_RATIO_MEASURE(7850.),#3399);
#3419=PROPERTY_DEFINITION_REPRESENTATION(#3514,#3457);
#3420=PROPERTY_DEFINITION_REPRESENTATION(#3515,#3458);
#3421=PROPERTY_DEFINITION_REPRESENTATION(#3516,#3459);
#3422=PROPERTY_DEFINITION_REPRESENTATION(#3517,#3460);
#3423=PROPERTY_DEFINITION_REPRESENTATION(#3518,#3461);
#3424=PROPERTY_DEFINITION_REPRESENTATION(#3519,#3462);
#3425=PROPERTY_DEFINITION_REPRESENTATION(#3520,#3463);
#3426=PROPERTY_DEFINITION_REPRESENTATION(#3521,#3464);
#3427=PROPERTY_DEFINITION_REPRESENTATION(#3522,#3465);
#3428=PROPERTY_DEFINITION_REPRESENTATION(#3523,#3466);
#3429=PROPERTY_DEFINITION_REPRESENTATION(#3524,#3467);
#3430=PROPERTY_DEFINITION_REPRESENTATION(#3525,#3468);
#3431=PROPERTY_DEFINITION_REPRESENTATION(#3526,#3469);
#3432=PROPERTY_DEFINITION_REPRESENTATION(#3527,#3470);
#3433=PROPERTY_DEFINITION_REPRESENTATION(#3528,#3471);
#3434=PROPERTY_DEFINITION_REPRESENTATION(#3529,#3472);
#3435=PROPERTY_DEFINITION_REPRESENTATION(#3530,#3473);
#3436=PROPERTY_DEFINITION_REPRESENTATION(#3531,#3474);
#3437=PROPERTY_DEFINITION_REPRESENTATION(#3532,#3475);
#3438=PROPERTY_DEFINITION_REPRESENTATION(#3533,#3476);
#3439=PROPERTY_DEFINITION_REPRESENTATION(#3534,#3477);
#3440=PROPERTY_DEFINITION_REPRESENTATION(#3535,#3478);
#3441=PROPERTY_DEFINITION_REPRESENTATION(#3536,#3479);
#3442=PROPERTY_DEFINITION_REPRESENTATION(#3537,#3480);
#3443=PROPERTY_DEFINITION_REPRESENTATION(#3538,#3481);
#3444=PROPERTY_DEFINITION_REPRESENTATION(#3539,#3482);
#3445=PROPERTY_DEFINITION_REPRESENTATION(#3540,#3483);
#3446=PROPERTY_DEFINITION_REPRESENTATION(#3541,#3484);
#3447=PROPERTY_DEFINITION_REPRESENTATION(#3542,#3485);
#3448=PROPERTY_DEFINITION_REPRESENTATION(#3543,#3486);
#3449=PROPERTY_DEFINITION_REPRESENTATION(#3544,#3487);
#3450=PROPERTY_DEFINITION_REPRESENTATION(#3545,#3488);
#3451=PROPERTY_DEFINITION_REPRESENTATION(#3546,#3489);
#3452=PROPERTY_DEFINITION_REPRESENTATION(#3547,#3490);
#3453=PROPERTY_DEFINITION_REPRESENTATION(#3548,#3491);
#3454=PROPERTY_DEFINITION_REPRESENTATION(#3549,#3492);
#3455=PROPERTY_DEFINITION_REPRESENTATION(#3550,#3493);
#3456=PROPERTY_DEFINITION_REPRESENTATION(#3551,#3494);
#3457=REPRESENTATION('material name',(#3495),#6783);
#3458=REPRESENTATION('density',(#3400),#6783);
#3459=REPRESENTATION('material name',(#3496),#6784);
#3460=REPRESENTATION('density',(#3401),#6784);
#3461=REPRESENTATION('material name',(#3497),#6785);
#3462=REPRESENTATION('density',(#3402),#6785);
#3463=REPRESENTATION('material name',(#3498),#6786);
#3464=REPRESENTATION('density',(#3403),#6786);
#3465=REPRESENTATION('material name',(#3499),#6787);
#3466=REPRESENTATION('density',(#3404),#6787);
#3467=REPRESENTATION('material name',(#3500),#6788);
#3468=REPRESENTATION('density',(#3405),#6788);
#3469=REPRESENTATION('material name',(#3501),#6789);
#3470=REPRESENTATION('density',(#3406),#6789);
#3471=REPRESENTATION('material name',(#3502),#6790);
#3472=REPRESENTATION('density',(#3407),#6790);
#3473=REPRESENTATION('material name',(#3503),#6791);
#3474=REPRESENTATION('density',(#3408),#6791);
#3475=REPRESENTATION('material name',(#3504),#6793);
#3476=REPRESENTATION('density',(#3409),#6793);
#3477=REPRESENTATION('material name',(#3505),#6794);
#3478=REPRESENTATION('density',(#3410),#6794);
#3479=REPRESENTATION('material name',(#3506),#6795);
#3480=REPRESENTATION('density',(#3411),#6795);
#3481=REPRESENTATION('material name',(#3507),#6796);
#3482=REPRESENTATION('density',(#3412),#6796);
#3483=REPRESENTATION('material name',(#3508),#6798);
#3484=REPRESENTATION('density',(#3413),#6798);
#3485=REPRESENTATION('material name',(#3509),#6800);
#3486=REPRESENTATION('density',(#3414),#6800);
#3487=REPRESENTATION('material name',(#3510),#6801);
#3488=REPRESENTATION('density',(#3415),#6801);
#3489=REPRESENTATION('material name',(#3511),#6802);
#3490=REPRESENTATION('density',(#3416),#6802);
#3491=REPRESENTATION('material name',(#3512),#6803);
#3492=REPRESENTATION('density',(#3417),#6803);
#3493=REPRESENTATION('material name',(#3513),#6804);
#3494=REPRESENTATION('density',(#3418),#6804);
#3495=DESCRIPTIVE_REPRESENTATION_ITEM('Steel','Steel');
#3496=DESCRIPTIVE_REPRESENTATION_ITEM('Steel','Steel');
#3497=DESCRIPTIVE_REPRESENTATION_ITEM('Steel','Steel');
#3498=DESCRIPTIVE_REPRESENTATION_ITEM('Steel','Steel');
#3499=DESCRIPTIVE_REPRESENTATION_ITEM('Steel','Steel');
#3500=DESCRIPTIVE_REPRESENTATION_ITEM('Steel','Steel');
#3501=DESCRIPTIVE_REPRESENTATION_ITEM('Steel','Steel');
#3502=DESCRIPTIVE_REPRESENTATION_ITEM('Steel','Steel');
#3503=DESCRIPTIVE_REPRESENTATION_ITEM('Steel','Steel');
#3504=DESCRIPTIVE_REPRESENTATION_ITEM('Steel','Steel');
#3505=DESCRIPTIVE_REPRESENTATION_ITEM('Steel','Steel');
#3506=DESCRIPTIVE_REPRESENTATION_ITEM('Steel','Steel');
#3507=DESCRIPTIVE_REPRESENTATION_ITEM('Steel','Steel');
#3508=DESCRIPTIVE_REPRESENTATION_ITEM('Steel','Steel');
#3509=DESCRIPTIVE_REPRESENTATION_ITEM('Steel','Steel');
#3510=DESCRIPTIVE_REPRESENTATION_ITEM('Steel','Steel');
#3511=DESCRIPTIVE_REPRESENTATION_ITEM('Steel','Steel');
#3512=DESCRIPTIVE_REPRESENTATION_ITEM('Steel','Steel');
#3513=DESCRIPTIVE_REPRESENTATION_ITEM('Steel','Steel');
#3514=PROPERTY_DEFINITION('material property','material name',#6925);
#3515=PROPERTY_DEFINITION('material property','density of part',#6925);
#3516=PROPERTY_DEFINITION('material property','material name',#6926);
#3517=PROPERTY_DEFINITION('material property','density of part',#6926);
#3518=PROPERTY_DEFINITION('material property','material name',#6927);
#3519=PROPERTY_DEFINITION('material property','density of part',#6927);
#3520=PROPERTY_DEFINITION('material property','material name',#6928);
#3521=PROPERTY_DEFINITION('material property','density of part',#6928);
#3522=PROPERTY_DEFINITION('material property','material name',#6929);
#3523=PROPERTY_DEFINITION('material property','density of part',#6929);
#3524=PROPERTY_DEFINITION('material property','material name',#6930);
#3525=PROPERTY_DEFINITION('material property','density of part',#6930);
#3526=PROPERTY_DEFINITION('material property','material name',#6931);
#3527=PROPERTY_DEFINITION('material property','density of part',#6931);
#3528=PROPERTY_DEFINITION('material property','material name',#6932);
#3529=PROPERTY_DEFINITION('material property','density of part',#6932);
#3530=PROPERTY_DEFINITION('material property','material name',#6933);
#3531=PROPERTY_DEFINITION('material property','density of part',#6933);
#3532=PROPERTY_DEFINITION('material property','material name',#6935);
#3533=PROPERTY_DEFINITION('material property','density of part',#6935);
#3534=PROPERTY_DEFINITION('material property','material name',#6936);
#3535=PROPERTY_DEFINITION('material property','density of part',#6936);
#3536=PROPERTY_DEFINITION('material property','material name',#6937);
#3537=PROPERTY_DEFINITION('material property','density of part',#6937);
#3538=PROPERTY_DEFINITION('material property','material name',#6938);
#3539=PROPERTY_DEFINITION('material property','density of part',#6938);
#3540=PROPERTY_DEFINITION('material property','material name',#6940);
#3541=PROPERTY_DEFINITION('material property','density of part',#6940);
#3542=PROPERTY_DEFINITION('material property','material name',#6942);
#3543=PROPERTY_DEFINITION('material property','density of part',#6942);
#3544=PROPERTY_DEFINITION('material property','material name',#6943);
#3545=PROPERTY_DEFINITION('material property','density of part',#6943);
#3546=PROPERTY_DEFINITION('material property','material name',#6944);
#3547=PROPERTY_DEFINITION('material property','density of part',#6944);
#3548=PROPERTY_DEFINITION('material property','material name',#6945);
#3549=PROPERTY_DEFINITION('material property','density of part',#6945);
#3550=PROPERTY_DEFINITION('material property','material name',#6946);
#3551=PROPERTY_DEFINITION('material property','density of part',#6946);
#3552=AXIS2_PLACEMENT_3D('',#4932,#3936,#3937);
#3553=AXIS2_PLACEMENT_3D('',#4933,#3938,#3939);
#3554=AXIS2_PLACEMENT_3D('',#4934,#3940,#3941);
#3555=AXIS2_PLACEMENT_3D('',#4935,#3942,#3943);
#3556=AXIS2_PLACEMENT_3D('',#4937,#3944,#3945);
#3557=AXIS2_PLACEMENT_3D('',#4940,#3947,#3948);
#3558=AXIS2_PLACEMENT_3D('',#4941,#3949,#3950);
#3559=AXIS2_PLACEMENT_3D('',#4943,#3951,#3952);
#3560=AXIS2_PLACEMENT_3D('',#4946,#3954,#3955);
#3561=AXIS2_PLACEMENT_3D('',#4947,#3956,#3957);
#3562=AXIS2_PLACEMENT_3D('',#4949,#3958,#3959);
#3563=AXIS2_PLACEMENT_3D('',#4952,#3961,#3962);
#3564=AXIS2_PLACEMENT_3D('',#4953,#3963,#3964);
#3565=AXIS2_PLACEMENT_3D('',#4955,#3965,#3966);
#3566=AXIS2_PLACEMENT_3D('',#4958,#3968,#3969);
#3567=AXIS2_PLACEMENT_3D('',#4959,#3970,#3971);
#3568=AXIS2_PLACEMENT_3D('',#4961,#3972,#3973);
#3569=AXIS2_PLACEMENT_3D('',#4964,#3975,#3976);
#3570=AXIS2_PLACEMENT_3D('',#4965,#3977,#3978);
#3571=AXIS2_PLACEMENT_3D('',#4974,#3983,#3984);
#3572=AXIS2_PLACEMENT_3D('',#4983,#3989,#3990);
#3573=AXIS2_PLACEMENT_3D('',#4986,#3993,#3994);
#3574=AXIS2_PLACEMENT_3D('',#4988,#3996,#3997);
#3575=AXIS2_PLACEMENT_3D('',#4990,#3999,#4000);
#3576=AXIS2_PLACEMENT_3D('',#4992,#4001,#4002);
#3577=AXIS2_PLACEMENT_3D('',#4995,#4004,#4005);
#3578=AXIS2_PLACEMENT_3D('',#4996,#4006,#4007);
#3579=AXIS2_PLACEMENT_3D('',#4998,#4008,#4009);
#3580=AXIS2_PLACEMENT_3D('',#5001,#4011,#4012);
#3581=AXIS2_PLACEMENT_3D('',#5002,#4013,#4014);
#3582=AXIS2_PLACEMENT_3D('',#5004,#4015,#4016);
#3583=AXIS2_PLACEMENT_3D('',#5007,#4018,#4019);
#3584=AXIS2_PLACEMENT_3D('',#5008,#4020,#4021);
#3585=AXIS2_PLACEMENT_3D('',#5010,#4022,#4023);
#3586=AXIS2_PLACEMENT_3D('',#5013,#4025,#4026);
#3587=AXIS2_PLACEMENT_3D('',#5014,#4027,#4028);
#3588=AXIS2_PLACEMENT_3D('',#5016,#4029,#4030);
#3589=AXIS2_PLACEMENT_3D('',#5019,#4032,#4033);
#3590=AXIS2_PLACEMENT_3D('',#5020,#4034,#4035);
#3591=AXIS2_PLACEMENT_3D('',#5029,#4040,#4041);
#3592=AXIS2_PLACEMENT_3D('',#5038,#4046,#4047);
#3593=AXIS2_PLACEMENT_3D('',#5041,#4050,#4051);
#3594=AXIS2_PLACEMENT_3D('',#5043,#4053,#4054);
#3595=AXIS2_PLACEMENT_3D('',#5045,#4056,#4057);
#3596=AXIS2_PLACEMENT_3D('',#5054,#4062,#4063);
#3597=AXIS2_PLACEMENT_3D('',#5060,#4067,#4068);
#3598=AXIS2_PLACEMENT_3D('',#5066,#4072,#4073);
#3599=AXIS2_PLACEMENT_3D('',#5069,#4076,#4077);
#3600=AXIS2_PLACEMENT_3D('',#5070,#4078,#4079);
#3601=AXIS2_PLACEMENT_3D('',#5071,#4080,#4081);
#3602=AXIS2_PLACEMENT_3D('',#5072,#4082,#4083);
#3603=AXIS2_PLACEMENT_3D('',#5074,#4084,#4085);
#3604=AXIS2_PLACEMENT_3D('',#5077,#4087,#4088);
#3605=AXIS2_PLACEMENT_3D('',#5078,#4089,#4090);
#3606=AXIS2_PLACEMENT_3D('',#5080,#4091,#4092);
#3607=AXIS2_PLACEMENT_3D('',#5083,#4094,#4095);
#3608=AXIS2_PLACEMENT_3D('',#5084,#4096,#4097);
#3609=AXIS2_PLACEMENT_3D('',#5085,#4098,#4099);
#3610=AXIS2_PLACEMENT_3D('',#5086,#4100,#4101);
#3611=AXIS2_PLACEMENT_3D('',#5087,#4102,#4103);
#3612=AXIS2_PLACEMENT_3D('',#5089,#4104,#4105);
#3613=AXIS2_PLACEMENT_3D('',#5092,#4107,#4108);
#3614=AXIS2_PLACEMENT_3D('',#5093,#4109,#4110);
#3615=AXIS2_PLACEMENT_3D('',#5095,#4111,#4112);
#3616=AXIS2_PLACEMENT_3D('',#5098,#4114,#4115);
#3617=AXIS2_PLACEMENT_3D('',#5099,#4116,#4117);
#3618=AXIS2_PLACEMENT_3D('',#5100,#4118,#4119);
#3619=AXIS2_PLACEMENT_3D('',#5101,#4120,#4121);
#3620=AXIS2_PLACEMENT_3D('',#5102,#4122,#4123);
#3621=AXIS2_PLACEMENT_3D('',#5104,#4124,#4125);
#3622=AXIS2_PLACEMENT_3D('',#5107,#4127,#4128);
#3623=AXIS2_PLACEMENT_3D('',#5108,#4129,#4130);
#3624=AXIS2_PLACEMENT_3D('',#5110,#4131,#4132);
#3625=AXIS2_PLACEMENT_3D('',#5113,#4134,#4135);
#3626=AXIS2_PLACEMENT_3D('',#5114,#4136,#4137);
#3627=AXIS2_PLACEMENT_3D('',#5115,#4138,#4139);
#3628=AXIS2_PLACEMENT_3D('',#5116,#4140,#4141);
#3629=AXIS2_PLACEMENT_3D('',#5117,#4142,#4143);
#3630=AXIS2_PLACEMENT_3D('',#5119,#4144,#4145);
#3631=AXIS2_PLACEMENT_3D('',#5122,#4147,#4148);
#3632=AXIS2_PLACEMENT_3D('',#5123,#4149,#4150);
#3633=AXIS2_PLACEMENT_3D('',#5125,#4151,#4152);
#3634=AXIS2_PLACEMENT_3D('',#5128,#4154,#4155);
#3635=AXIS2_PLACEMENT_3D('',#5129,#4156,#4157);
#3636=AXIS2_PLACEMENT_3D('',#5130,#4158,#4159);
#3637=AXIS2_PLACEMENT_3D('',#5131,#4160,#4161);
#3638=AXIS2_PLACEMENT_3D('',#5132,#4162,#4163);
#3639=AXIS2_PLACEMENT_3D('',#5134,#4164,#4165);
#3640=AXIS2_PLACEMENT_3D('',#5137,#4167,#4168);
#3641=AXIS2_PLACEMENT_3D('',#5138,#4169,#4170);
#3642=AXIS2_PLACEMENT_3D('',#5140,#4171,#4172);
#3643=AXIS2_PLACEMENT_3D('',#5143,#4174,#4175);
#3644=AXIS2_PLACEMENT_3D('',#5144,#4176,#4177);
#3645=AXIS2_PLACEMENT_3D('',#5145,#4178,#4179);
#3646=AXIS2_PLACEMENT_3D('',#5146,#4180,#4181);
#3647=AXIS2_PLACEMENT_3D('',#5147,#4182,#4183);
#3648=AXIS2_PLACEMENT_3D('',#5149,#4184,#4185);
#3649=AXIS2_PLACEMENT_3D('',#5152,#4187,#4188);
#3650=AXIS2_PLACEMENT_3D('',#5153,#4189,#4190);
#3651=AXIS2_PLACEMENT_3D('',#5155,#4191,#4192);
#3652=AXIS2_PLACEMENT_3D('',#5158,#4194,#4195);
#3653=AXIS2_PLACEMENT_3D('',#5159,#4196,#4197);
#3654=AXIS2_PLACEMENT_3D('',#5160,#4198,#4199);
#3655=AXIS2_PLACEMENT_3D('',#5161,#4200,#4201);
#3656=AXIS2_PLACEMENT_3D('',#5162,#4202,#4203);
#3657=AXIS2_PLACEMENT_3D('',#5164,#4204,#4205);
#3658=AXIS2_PLACEMENT_3D('',#5167,#4207,#4208);
#3659=AXIS2_PLACEMENT_3D('',#5168,#4209,#4210);
#3660=AXIS2_PLACEMENT_3D('',#5170,#4211,#4212);
#3661=AXIS2_PLACEMENT_3D('',#5173,#4214,#4215);
#3662=AXIS2_PLACEMENT_3D('',#5174,#4216,#4217);
#3663=AXIS2_PLACEMENT_3D('',#5175,#4218,#4219);
#3664=AXIS2_PLACEMENT_3D('',#5176,#4220,#4221);
#3665=AXIS2_PLACEMENT_3D('',#5177,#4222,#4223);
#3666=AXIS2_PLACEMENT_3D('',#5179,#4224,#4225);
#3667=AXIS2_PLACEMENT_3D('',#5182,#4227,#4228);
#3668=AXIS2_PLACEMENT_3D('',#5183,#4229,#4230);
#3669=AXIS2_PLACEMENT_3D('',#5185,#4231,#4232);
#3670=AXIS2_PLACEMENT_3D('',#5188,#4234,#4235);
#3671=AXIS2_PLACEMENT_3D('',#5189,#4236,#4237);
#3672=AXIS2_PLACEMENT_3D('',#5190,#4238,#4239);
#3673=AXIS2_PLACEMENT_3D('',#5191,#4240,#4241);
#3674=AXIS2_PLACEMENT_3D('',#5192,#4242,#4243);
#3675=AXIS2_PLACEMENT_3D('',#5193,#4244,#4245);
#3676=AXIS2_PLACEMENT_3D('',#5195,#4246,#4247);
#3677=AXIS2_PLACEMENT_3D('',#5198,#4249,#4250);
#3678=AXIS2_PLACEMENT_3D('',#5199,#4251,#4252);
#3679=AXIS2_PLACEMENT_3D('',#5201,#4253,#4254);
#3680=AXIS2_PLACEMENT_3D('',#5204,#4256,#4257);
#3681=AXIS2_PLACEMENT_3D('',#5205,#4258,#4259);
#3682=AXIS2_PLACEMENT_3D('',#5208,#4260,#4261);
#3683=AXIS2_PLACEMENT_3D('',#5209,#4262,#4263);
#3684=AXIS2_PLACEMENT_3D('',#5211,#4264,#4265);
#3685=AXIS2_PLACEMENT_3D('',#5214,#4267,#4268);
#3686=AXIS2_PLACEMENT_3D('',#5215,#4269,#4270);
#3687=AXIS2_PLACEMENT_3D('',#5217,#4271,#4272);
#3688=AXIS2_PLACEMENT_3D('',#5220,#4274,#4275);
#3689=AXIS2_PLACEMENT_3D('',#5221,#4276,#4277);
#3690=AXIS2_PLACEMENT_3D('',#5222,#4278,#4279);
#3691=AXIS2_PLACEMENT_3D('',#5223,#4280,#4281);
#3692=AXIS2_PLACEMENT_3D('',#5225,#4282,#4283);
#3693=AXIS2_PLACEMENT_3D('',#5228,#4285,#4286);
#3694=AXIS2_PLACEMENT_3D('',#5229,#4287,#4288);
#3695=AXIS2_PLACEMENT_3D('',#5231,#4289,#4290);
#3696=AXIS2_PLACEMENT_3D('',#5234,#4292,#4293);
#3697=AXIS2_PLACEMENT_3D('',#5235,#4294,#4295);
#3698=AXIS2_PLACEMENT_3D('',#5237,#4296,#4297);
#3699=AXIS2_PLACEMENT_3D('',#5240,#4299,#4300);
#3700=AXIS2_PLACEMENT_3D('',#5241,#4301,#4302);
#3701=AXIS2_PLACEMENT_3D('',#5243,#4303,#4304);
#3702=AXIS2_PLACEMENT_3D('',#5246,#4306,#4307);
#3703=AXIS2_PLACEMENT_3D('',#5247,#4308,#4309);
#3704=AXIS2_PLACEMENT_3D('',#5256,#4314,#4315);
#3705=AXIS2_PLACEMENT_3D('',#5262,#4319,#4320);
#3706=AXIS2_PLACEMENT_3D('',#5268,#4324,#4325);
#3707=AXIS2_PLACEMENT_3D('',#5274,#4329,#4330);
#3708=AXIS2_PLACEMENT_3D('',#5280,#4334,#4335);
#3709=AXIS2_PLACEMENT_3D('',#5286,#4339,#4340);
#3710=AXIS2_PLACEMENT_3D('',#5292,#4344,#4345);
#3711=AXIS2_PLACEMENT_3D('',#5295,#4348,#4349);
#3712=AXIS2_PLACEMENT_3D('',#5296,#4350,#4351);
#3713=AXIS2_PLACEMENT_3D('',#5297,#4352,#4353);
#3714=AXIS2_PLACEMENT_3D('',#5298,#4354,#4355);
#3715=AXIS2_PLACEMENT_3D('',#5300,#4356,#4357);
#3716=AXIS2_PLACEMENT_3D('',#5303,#4359,#4360);
#3717=AXIS2_PLACEMENT_3D('',#5304,#4361,#4362);
#3718=AXIS2_PLACEMENT_3D('',#5306,#4363,#4364);
#3719=AXIS2_PLACEMENT_3D('',#5307,#4365,#4366);
#3720=AXIS2_PLACEMENT_3D('',#5310,#4367,#4368);
#3721=AXIS2_PLACEMENT_3D('',#5312,#4369,#4370);
#3722=AXIS2_PLACEMENT_3D('',#5313,#4371,#4372);
#3723=AXIS2_PLACEMENT_3D('',#5314,#4373,#4374);
#3724=AXIS2_PLACEMENT_3D('',#5392,#4376,#4377);
#3725=AXIS2_PLACEMENT_3D('',#5470,#4379,#4380);
#3726=AXIS2_PLACEMENT_3D('',#5472,#4381,#4382);
#3727=AXIS2_PLACEMENT_3D('',#5475,#4384,#4385);
#3728=AXIS2_PLACEMENT_3D('',#5640,#4386,#4387);
#3729=AXIS2_PLACEMENT_3D('',#5677,#4389,#4390);
#3730=AXIS2_PLACEMENT_3D('',#5714,#4392,#4393);
#3731=AXIS2_PLACEMENT_3D('',#5751,#4395,#4396);
#3732=AXIS2_PLACEMENT_3D('',#5788,#4398,#4399);
#3733=AXIS2_PLACEMENT_3D('',#5790,#4400,#4401);
#3734=AXIS2_PLACEMENT_3D('',#5791,#4402,#4403);
#3735=AXIS2_PLACEMENT_3D('',#5793,#4404,#4405);
#3736=AXIS2_PLACEMENT_3D('',#5794,#4406,#4407);
#3737=AXIS2_PLACEMENT_3D('',#5796,#4408,#4409);
#3738=AXIS2_PLACEMENT_3D('',#5798,#4411,#4412);
#3739=AXIS2_PLACEMENT_3D('',#5800,#4413,#4414);
#3740=AXIS2_PLACEMENT_3D('',#5801,#4415,#4416);
#3741=AXIS2_PLACEMENT_3D('',#5803,#4418,#4419);
#3742=AXIS2_PLACEMENT_3D('',#5804,#4420,#4421);
#3743=AXIS2_PLACEMENT_3D('',#5805,#4422,#4423);
#3744=AXIS2_PLACEMENT_3D('',#5806,#4424,#4425);
#3745=AXIS2_PLACEMENT_3D('',#5808,#4426,#4427);
#3746=AXIS2_PLACEMENT_3D('',#5811,#4429,#4430);
#3747=AXIS2_PLACEMENT_3D('',#5812,#4431,#4432);
#3748=AXIS2_PLACEMENT_3D('',#5814,#4433,#4434);
#3749=AXIS2_PLACEMENT_3D('',#5817,#4436,#4437);
#3750=AXIS2_PLACEMENT_3D('',#5818,#4438,#4439);
#3751=AXIS2_PLACEMENT_3D('',#5819,#4440,#4441);
#3752=AXIS2_PLACEMENT_3D('',#5820,#4442,#4443);
#3753=AXIS2_PLACEMENT_3D('',#5821,#4444,#4445);
#3754=AXIS2_PLACEMENT_3D('',#5823,#4446,#4447);
#3755=AXIS2_PLACEMENT_3D('',#5824,#4448,#4449);
#3756=AXIS2_PLACEMENT_3D('',#5826,#4450,#4451);
#3757=AXIS2_PLACEMENT_3D('',#5828,#4453,#4454);
#3758=AXIS2_PLACEMENT_3D('',#5830,#4455,#4456);
#3759=AXIS2_PLACEMENT_3D('',#5832,#4458,#4459);
#3760=AXIS2_PLACEMENT_3D('',#5834,#4460,#4461);
#3761=AXIS2_PLACEMENT_3D('',#5836,#4463,#4464);
#3762=AXIS2_PLACEMENT_3D('',#5838,#4465,#4466);
#3763=AXIS2_PLACEMENT_3D('',#5839,#4467,#4468);
#3764=AXIS2_PLACEMENT_3D('',#5841,#4469,#4470);
#3765=AXIS2_PLACEMENT_3D('',#5843,#4472,#4473);
#3766=AXIS2_PLACEMENT_3D('',#5845,#4474,#4475);
#3767=AXIS2_PLACEMENT_3D('',#5847,#4477,#4478);
#3768=AXIS2_PLACEMENT_3D('',#5849,#4479,#4480);
#3769=AXIS2_PLACEMENT_3D('',#5851,#4482,#4483);
#3770=AXIS2_PLACEMENT_3D('',#5852,#4484,#4485);
#3771=AXIS2_PLACEMENT_3D('',#5861,#4490,#4491);
#3772=AXIS2_PLACEMENT_3D('',#5867,#4495,#4496);
#3773=AXIS2_PLACEMENT_3D('',#5873,#4500,#4501);
#3774=AXIS2_PLACEMENT_3D('',#5879,#4505,#4506);
#3775=AXIS2_PLACEMENT_3D('',#5885,#4510,#4511);
#3776=AXIS2_PLACEMENT_3D('',#5888,#4514,#4515);
#3777=AXIS2_PLACEMENT_3D('',#5889,#4516,#4517);
#3778=AXIS2_PLACEMENT_3D('',#5890,#4518,#4519);
#3779=AXIS2_PLACEMENT_3D('',#5891,#4520,#4521);
#3780=AXIS2_PLACEMENT_3D('',#5892,#4522,#4523);
#3781=AXIS2_PLACEMENT_3D('',#5893,#4524,#4525);
#3782=AXIS2_PLACEMENT_3D('',#5894,#4526,#4527);
#3783=AXIS2_PLACEMENT_3D('',#5895,#4528,#4529);
#3784=AXIS2_PLACEMENT_3D('',#5896,#4530,#4531);
#3785=AXIS2_PLACEMENT_3D('',#5897,#4532,#4533);
#3786=AXIS2_PLACEMENT_3D('',#5898,#4534,#4535);
#3787=AXIS2_PLACEMENT_3D('',#5899,#4536,#4537);
#3788=AXIS2_PLACEMENT_3D('',#5900,#4538,#4539);
#3789=AXIS2_PLACEMENT_3D('',#5901,#4540,#4541);
#3790=AXIS2_PLACEMENT_3D('',#5902,#4542,#4543);
#3791=AXIS2_PLACEMENT_3D('',#5903,#4544,#4545);
#3792=AXIS2_PLACEMENT_3D('',#5904,#4546,#4547);
#3793=AXIS2_PLACEMENT_3D('',#5905,#4548,#4549);
#3794=AXIS2_PLACEMENT_3D('',#5906,#4550,#4551);
#3795=AXIS2_PLACEMENT_3D('',#5907,#4552,#4553);
#3796=AXIS2_PLACEMENT_3D('',#5908,#4554,#4555);
#3797=AXIS2_PLACEMENT_3D('',#5909,#4556,#4557);
#3798=AXIS2_PLACEMENT_3D('',#5910,#4558,#4559);
#3799=AXIS2_PLACEMENT_3D('',#5911,#4560,#4561);
#3800=AXIS2_PLACEMENT_3D('',#5912,#4562,#4563);
#3801=AXIS2_PLACEMENT_3D('',#5913,#4564,#4565);
#3802=AXIS2_PLACEMENT_3D('',#5914,#4566,#4567);
#3803=AXIS2_PLACEMENT_3D('',#5915,#4568,#4569);
#3804=AXIS2_PLACEMENT_3D('',#5916,#4570,#4571);
#3805=AXIS2_PLACEMENT_3D('',#5917,#4572,#4573);
#3806=AXIS2_PLACEMENT_3D('',#5918,#4574,#4575);
#3807=AXIS2_PLACEMENT_3D('',#5919,#4576,#4577);
#3808=AXIS2_PLACEMENT_3D('',#5928,#4582,#4583);
#3809=AXIS2_PLACEMENT_3D('',#5930,#4584,#4585);
#3810=AXIS2_PLACEMENT_3D('',#5934,#4588,#4589);
#3811=AXIS2_PLACEMENT_3D('',#5938,#4592,#4593);
#3812=AXIS2_PLACEMENT_3D('',#5942,#4596,#4597);
#3813=AXIS2_PLACEMENT_3D('',#5943,#4598,#4599);
#3814=AXIS2_PLACEMENT_3D('',#5944,#4600,#4601);
#3815=AXIS2_PLACEMENT_3D('',#5946,#4602,#4603);
#3816=AXIS2_PLACEMENT_3D('',#5949,#4605,#4606);
#3817=AXIS2_PLACEMENT_3D('',#5950,#4607,#4608);
#3818=AXIS2_PLACEMENT_3D('',#5951,#4609,#4610);
#3819=AXIS2_PLACEMENT_3D('',#5952,#4611,#4612);
#3820=AXIS2_PLACEMENT_3D('',#5953,#4613,#4614);
#3821=AXIS2_PLACEMENT_3D('',#5954,#4615,#4616);
#3822=AXIS2_PLACEMENT_3D('',#5956,#4617,#4618);
#3823=AXIS2_PLACEMENT_3D('',#5957,#4619,#4620);
#3824=AXIS2_PLACEMENT_3D('',#5959,#4621,#4622);
#3825=AXIS2_PLACEMENT_3D('',#5961,#4624,#4625);
#3826=AXIS2_PLACEMENT_3D('',#5963,#4626,#4627);
#3827=AXIS2_PLACEMENT_3D('',#5965,#4629,#4630);
#3828=AXIS2_PLACEMENT_3D('',#5967,#4631,#4632);
#3829=AXIS2_PLACEMENT_3D('',#5968,#4633,#4634);
#3830=AXIS2_PLACEMENT_3D('',#5970,#4635,#4636);
#3831=AXIS2_PLACEMENT_3D('',#5972,#4638,#4639);
#3832=AXIS2_PLACEMENT_3D('',#5973,#4640,#4641);
#3833=AXIS2_PLACEMENT_3D('',#6091,#4643,#4644);
#3834=AXIS2_PLACEMENT_3D('',#6175,#4646,#4647);
#3835=AXIS2_PLACEMENT_3D('',#6184,#4652,#4653);
#3836=AXIS2_PLACEMENT_3D('',#6193,#4658,#4659);
#3837=AXIS2_PLACEMENT_3D('',#6196,#4662,#4663);
#3838=AXIS2_PLACEMENT_3D('',#6198,#4664,#4665);
#3839=AXIS2_PLACEMENT_3D('',#6199,#4666,#4667);
#3840=AXIS2_PLACEMENT_3D('',#6200,#4668,#4669);
#3841=AXIS2_PLACEMENT_3D('',#6201,#4670,#4671);
#3842=AXIS2_PLACEMENT_3D('',#6202,#4672,#4673);
#3843=AXIS2_PLACEMENT_3D('',#6292,#4675,#4676);
#3844=AXIS2_PLACEMENT_3D('',#6382,#4678,#4679);
#3845=AXIS2_PLACEMENT_3D('',#6470,#4681,#4682);
#3846=AXIS2_PLACEMENT_3D('',#6472,#4683,#4684);
#3847=AXIS2_PLACEMENT_3D('',#6473,#4685,#4686);
#3848=AXIS2_PLACEMENT_3D('',#6476,#4689,#4690);
#3849=AXIS2_PLACEMENT_3D('',#6478,#4691,#4692);
#3850=AXIS2_PLACEMENT_3D('',#6479,#4693,#4694);
#3851=AXIS2_PLACEMENT_3D('',#6480,#4695,#4696);
#3852=AXIS2_PLACEMENT_3D('',#6481,#4697,#4698);
#3853=AXIS2_PLACEMENT_3D('',#6482,#4699,#4700);
#3854=AXIS2_PLACEMENT_3D('',#6483,#4701,#4702);
#3855=AXIS2_PLACEMENT_3D('',#6484,#4703,#4704);
#3856=AXIS2_PLACEMENT_3D('',#6485,#4705,#4706);
#3857=AXIS2_PLACEMENT_3D('',#6494,#4711,#4712);
#3858=AXIS2_PLACEMENT_3D('',#6498,#4714,#4715);
#3859=AXIS2_PLACEMENT_3D('',#6499,#4716,#4717);
#3860=AXIS2_PLACEMENT_3D('',#6500,#4718,#4719);
#3861=AXIS2_PLACEMENT_3D('',#6506,#4723,#4724);
#3862=AXIS2_PLACEMENT_3D('',#6507,#4725,#4726);
#3863=AXIS2_PLACEMENT_3D('',#6508,#4727,#4728);
#3864=AXIS2_PLACEMENT_3D('',#6509,#4729,#4730);
#3865=AXIS2_PLACEMENT_3D('',#6513,#4732,#4733);
#3866=AXIS2_PLACEMENT_3D('',#6515,#4735,#4736);
#3867=AXIS2_PLACEMENT_3D('',#6519,#4739,#4740);
#3868=AXIS2_PLACEMENT_3D('',#6520,#4741,#4742);
#3869=AXIS2_PLACEMENT_3D('',#6526,#4746,#4747);
#3870=AXIS2_PLACEMENT_3D('',#6529,#4749,#4750);
#3871=AXIS2_PLACEMENT_3D('',#6530,#4751,#4752);
#3872=AXIS2_PLACEMENT_3D('',#6536,#4756,#4757);
#3873=AXIS2_PLACEMENT_3D('',#6537,#4758,#4759);
#3874=AXIS2_PLACEMENT_3D('',#6538,#4760,#4761);
#3875=AXIS2_PLACEMENT_3D('',#6539,#4762,#4763);
#3876=AXIS2_PLACEMENT_3D('',#6541,#4765,#4766);
#3877=AXIS2_PLACEMENT_3D('',#6542,#4767,#4768);
#3878=AXIS2_PLACEMENT_3D('',#6543,#4769,#4770);
#3879=AXIS2_PLACEMENT_3D('',#6544,#4771,#4772);
#3880=AXIS2_PLACEMENT_3D('',#6553,#4777,#4778);
#3881=AXIS2_PLACEMENT_3D('',#6559,#4782,#4783);
#3882=AXIS2_PLACEMENT_3D('',#6565,#4787,#4788);
#3883=AXIS2_PLACEMENT_3D('',#6571,#4792,#4793);
#3884=AXIS2_PLACEMENT_3D('',#6577,#4797,#4798);
#3885=AXIS2_PLACEMENT_3D('',#6580,#4801,#4802);
#3886=AXIS2_PLACEMENT_3D('',#6581,#4803,#4804);
#3887=AXIS2_PLACEMENT_3D('',#6583,#4805,#4806);
#3888=AXIS2_PLACEMENT_3D('',#6584,#4807,#4808);
#3889=AXIS2_PLACEMENT_3D('',#6586,#4809,#4810);
#3890=AXIS2_PLACEMENT_3D('',#6588,#4812,#4813);
#3891=AXIS2_PLACEMENT_3D('',#6590,#4814,#4815);
#3892=AXIS2_PLACEMENT_3D('',#6592,#4817,#4818);
#3893=AXIS2_PLACEMENT_3D('',#6594,#4819,#4820);
#3894=AXIS2_PLACEMENT_3D('',#6596,#4822,#4823);
#3895=AXIS2_PLACEMENT_3D('',#6597,#4824,#4825);
#3896=AXIS2_PLACEMENT_3D('',#6598,#4826,#4827);
#3897=AXIS2_PLACEMENT_3D('',#6670,#4829,#4830);
#3898=AXIS2_PLACEMENT_3D('',#6672,#4831,#4832);
#3899=AXIS2_PLACEMENT_3D('',#6674,#4833,#4834);
#3900=AXIS2_PLACEMENT_3D('',#6675,#4835,#4836);
#3901=AXIS2_PLACEMENT_3D('',#6677,#4837,#4838);
#3902=AXIS2_PLACEMENT_3D('',#6679,#4840,#4841);
#3903=AXIS2_PLACEMENT_3D('',#6681,#4842,#4843);
#3904=AXIS2_PLACEMENT_3D('',#6683,#4845,#4846);
#3905=AXIS2_PLACEMENT_3D('',#6685,#4847,#4848);
#3906=AXIS2_PLACEMENT_3D('',#6687,#4850,#4851);
#3907=AXIS2_PLACEMENT_3D('',#6689,#4852,#4853);
#3908=AXIS2_PLACEMENT_3D('',#6690,#4854,#4855);
#3909=AXIS2_PLACEMENT_3D('',#6692,#4857,#4858);
#3910=AXIS2_PLACEMENT_3D('',#6693,#4859,#4860);
#3911=AXIS2_PLACEMENT_3D('',#6702,#4865,#4866);
#3912=AXIS2_PLACEMENT_3D('',#6708,#4870,#4871);
#3913=AXIS2_PLACEMENT_3D('',#6714,#4875,#4876);
#3914=AXIS2_PLACEMENT_3D('',#6720,#4880,#4881);
#3915=AXIS2_PLACEMENT_3D('',#6726,#4885,#4886);
#3916=AXIS2_PLACEMENT_3D('',#6729,#4889,#4890);
#3917=AXIS2_PLACEMENT_3D('',#6730,#4891,#4892);
#3918=AXIS2_PLACEMENT_3D('',#6732,#4893,#4894);
#3919=AXIS2_PLACEMENT_3D('',#6733,#4895,#4896);
#3920=AXIS2_PLACEMENT_3D('',#6735,#4897,#4898);
#3921=AXIS2_PLACEMENT_3D('',#6737,#4900,#4901);
#3922=AXIS2_PLACEMENT_3D('',#6739,#4902,#4903);
#3923=AXIS2_PLACEMENT_3D('',#6741,#4905,#4906);
#3924=AXIS2_PLACEMENT_3D('',#6743,#4907,#4908);
#3925=AXIS2_PLACEMENT_3D('',#6745,#4910,#4911);
#3926=AXIS2_PLACEMENT_3D('',#6746,#4912,#4913);
#3927=AXIS2_PLACEMENT_3D('',#6747,#4914,#4915);
#3928=AXIS2_PLACEMENT_3D('',#6748,#4916,#4917);
#3929=AXIS2_PLACEMENT_3D('',#6749,#4918,#4919);
#3930=AXIS2_PLACEMENT_3D('',#6750,#4920,#4921);
#3931=AXIS2_PLACEMENT_3D('',#6751,#4922,#4923);
#3932=AXIS2_PLACEMENT_3D('',#6752,#4924,#4925);
#3933=AXIS2_PLACEMENT_3D('',#6753,#4926,#4927);
#3934=AXIS2_PLACEMENT_3D('',#6754,#4928,#4929);
#3935=AXIS2_PLACEMENT_3D('',#6755,#4930,#4931);
#3936=DIRECTION('axis',(0.,0.,1.));
#3937=DIRECTION('refdir',(1.,0.,0.));
#3938=DIRECTION('axis',(0.,0.,1.));
#3939=DIRECTION('refdir',(1.,0.,0.));
#3940=DIRECTION('axis',(0.,0.,1.));
#3941=DIRECTION('refdir',(1.,0.,0.));
#3942=DIRECTION('center_axis',(0.,1.,0.));
#3943=DIRECTION('ref_axis',(1.,0.,0.));
#3944=DIRECTION('center_axis',(0.,1.,0.));
#3945=DIRECTION('ref_axis',(1.,0.,0.));
#3946=DIRECTION('',(0.,1.,0.));
#3947=DIRECTION('center_axis',(0.,-1.,0.));
#3948=DIRECTION('ref_axis',(1.,0.,0.));
#3949=DIRECTION('center_axis',(0.,1.,0.));
#3950=DIRECTION('ref_axis',(1.,0.,0.));
#3951=DIRECTION('center_axis',(0.,1.,0.));
#3952=DIRECTION('ref_axis',(1.,0.,0.));
#3953=DIRECTION('',(0.,1.,0.));
#3954=DIRECTION('center_axis',(0.,-1.,0.));
#3955=DIRECTION('ref_axis',(1.,0.,0.));
#3956=DIRECTION('center_axis',(0.,1.,0.));
#3957=DIRECTION('ref_axis',(1.,0.,0.));
#3958=DIRECTION('center_axis',(0.,1.,0.));
#3959=DIRECTION('ref_axis',(1.,0.,0.));
#3960=DIRECTION('',(0.,1.,0.));
#3961=DIRECTION('center_axis',(0.,-1.,0.));
#3962=DIRECTION('ref_axis',(1.,0.,0.));
#3963=DIRECTION('center_axis',(0.,1.,0.));
#3964=DIRECTION('ref_axis',(1.,0.,0.));
#3965=DIRECTION('center_axis',(0.,1.,0.));
#3966=DIRECTION('ref_axis',(1.,0.,0.));
#3967=DIRECTION('',(0.,1.,0.));
#3968=DIRECTION('center_axis',(0.,-1.,0.));
#3969=DIRECTION('ref_axis',(1.,0.,0.));
#3970=DIRECTION('center_axis',(0.,1.,0.));
#3971=DIRECTION('ref_axis',(1.,0.,0.));
#3972=DIRECTION('center_axis',(0.,1.,0.));
#3973=DIRECTION('ref_axis',(1.,0.,0.));
#3974=DIRECTION('',(0.,1.,0.));
#3975=DIRECTION('center_axis',(0.,-1.,0.));
#3976=DIRECTION('ref_axis',(1.,0.,0.));
#3977=DIRECTION('center_axis',(-1.,0.,0.));
#3978=DIRECTION('ref_axis',(0.,0.,1.));
#3979=DIRECTION('',(0.,0.,-1.));
#3980=DIRECTION('',(0.,1.,0.));
#3981=DIRECTION('',(0.,0.,1.));
#3982=DIRECTION('',(0.,1.,0.));
#3983=DIRECTION('center_axis',(1.,0.,0.));
#3984=DIRECTION('ref_axis',(0.,0.,-1.));
#3985=DIRECTION('',(0.,0.,1.));
#3986=DIRECTION('',(0.,-1.,0.));
#3987=DIRECTION('',(0.,0.,-1.));
#3988=DIRECTION('',(0.,1.,0.));
#3989=DIRECTION('center_axis',(0.,0.,1.));
#3990=DIRECTION('ref_axis',(1.,0.,0.));
#3991=DIRECTION('',(-1.,0.,0.));
#3992=DIRECTION('',(1.,0.,0.));
#3993=DIRECTION('center_axis',(0.,1.,0.));
#3994=DIRECTION('ref_axis',(0.,0.,1.));
#3995=DIRECTION('',(1.,0.,0.));
#3996=DIRECTION('center_axis',(0.,1.,0.));
#3997=DIRECTION('ref_axis',(1.,0.,0.));
#3998=DIRECTION('',(-1.,0.,0.));
#3999=DIRECTION('center_axis',(0.,1.,0.));
#4000=DIRECTION('ref_axis',(1.,0.,0.));
#4001=DIRECTION('center_axis',(0.,1.,0.));
#4002=DIRECTION('ref_axis',(1.,0.,0.));
#4003=DIRECTION('',(0.,1.,0.));
#4004=DIRECTION('center_axis',(0.,-1.,0.));
#4005=DIRECTION('ref_axis',(1.,0.,0.));
#4006=DIRECTION('center_axis',(0.,1.,0.));
#4007=DIRECTION('ref_axis',(1.,0.,0.));
#4008=DIRECTION('center_axis',(0.,1.,0.));
#4009=DIRECTION('ref_axis',(1.,0.,0.));
#4010=DIRECTION('',(0.,1.,0.));
#4011=DIRECTION('center_axis',(0.,-1.,0.));
#4012=DIRECTION('ref_axis',(1.,0.,0.));
#4013=DIRECTION('center_axis',(0.,1.,0.));
#4014=DIRECTION('ref_axis',(1.,0.,0.));
#4015=DIRECTION('center_axis',(0.,1.,0.));
#4016=DIRECTION('ref_axis',(1.,0.,0.));
#4017=DIRECTION('',(0.,1.,0.));
#4018=DIRECTION('center_axis',(0.,-1.,0.));
#4019=DIRECTION('ref_axis',(1.,0.,0.));
#4020=DIRECTION('center_axis',(0.,1.,0.));
#4021=DIRECTION('ref_axis',(1.,0.,0.));
#4022=DIRECTION('center_axis',(0.,1.,0.));
#4023=DIRECTION('ref_axis',(1.,0.,0.));
#4024=DIRECTION('',(0.,1.,0.));
#4025=DIRECTION('center_axis',(0.,-1.,0.));
#4026=DIRECTION('ref_axis',(1.,0.,0.));
#4027=DIRECTION('center_axis',(0.,1.,0.));
#4028=DIRECTION('ref_axis',(1.,0.,0.));
#4029=DIRECTION('center_axis',(0.,1.,0.));
#4030=DIRECTION('ref_axis',(1.,0.,0.));
#4031=DIRECTION('',(0.,1.,0.));
#4032=DIRECTION('center_axis',(0.,-1.,0.));
#4033=DIRECTION('ref_axis',(1.,0.,0.));
#4034=DIRECTION('center_axis',(-1.,0.,0.));
#4035=DIRECTION('ref_axis',(0.,0.,1.));
#4036=DIRECTION('',(0.,0.,-1.));
#4037=DIRECTION('',(0.,1.,0.));
#4038=DIRECTION('',(0.,0.,1.));
#4039=DIRECTION('',(0.,1.,0.));
#4040=DIRECTION('center_axis',(1.,0.,0.));
#4041=DIRECTION('ref_axis',(0.,0.,-1.));
#4042=DIRECTION('',(0.,0.,1.));
#4043=DIRECTION('',(0.,-1.,0.));
#4044=DIRECTION('',(0.,0.,-1.));
#4045=DIRECTION('',(0.,1.,0.));
#4046=DIRECTION('center_axis',(0.,0.,1.));
#4047=DIRECTION('ref_axis',(1.,0.,0.));
#4048=DIRECTION('',(-1.,0.,0.));
#4049=DIRECTION('',(1.,0.,0.));
#4050=DIRECTION('center_axis',(0.,1.,0.));
#4051=DIRECTION('ref_axis',(0.,0.,1.));
#4052=DIRECTION('',(1.,0.,0.));
#4053=DIRECTION('center_axis',(0.,1.,0.));
#4054=DIRECTION('ref_axis',(1.,0.,0.));
#4055=DIRECTION('',(-1.,0.,0.));
#4056=DIRECTION('center_axis',(0.,1.,0.));
#4057=DIRECTION('ref_axis',(-1.,0.,0.));
#4058=DIRECTION('',(-1.,0.,0.));
#4059=DIRECTION('',(0.,0.,1.));
#4060=DIRECTION('',(-1.,0.,0.));
#4061=DIRECTION('',(0.,0.,1.));
#4062=DIRECTION('center_axis',(1.,0.,0.));
#4063=DIRECTION('ref_axis',(0.,1.,0.));
#4064=DIRECTION('',(0.,1.,0.));
#4065=DIRECTION('',(0.,1.,0.));
#4066=DIRECTION('',(0.,0.,1.));
#4067=DIRECTION('center_axis',(0.,-1.,0.));
#4068=DIRECTION('ref_axis',(1.,0.,0.));
#4069=DIRECTION('',(1.,0.,0.));
#4070=DIRECTION('',(1.,0.,0.));
#4071=DIRECTION('',(0.,0.,1.));
#4072=DIRECTION('center_axis',(-1.,0.,0.));
#4073=DIRECTION('ref_axis',(0.,-1.,0.));
#4074=DIRECTION('',(0.,-1.,0.));
#4075=DIRECTION('',(0.,-1.,0.));
#4076=DIRECTION('center_axis',(0.,0.,1.));
#4077=DIRECTION('ref_axis',(1.,0.,0.));
#4078=DIRECTION('center_axis',(0.,0.,1.));
#4079=DIRECTION('ref_axis',(1.,0.,0.));
#4080=DIRECTION('axis',(0.,0.,1.));
#4081=DIRECTION('refdir',(1.,0.,0.));
#4082=DIRECTION('center_axis',(0.,1.,0.));
#4083=DIRECTION('ref_axis',(1.,0.,0.));
#4084=DIRECTION('center_axis',(0.,-1.,0.));
#4085=DIRECTION('ref_axis',(1.,0.,0.));
#4086=DIRECTION('',(0.,-1.,0.));
#4087=DIRECTION('center_axis',(0.,-1.,0.));
#4088=DIRECTION('ref_axis',(1.,0.,0.));
#4089=DIRECTION('center_axis',(0.,1.,0.));
#4090=DIRECTION('ref_axis',(1.,0.,0.));
#4091=DIRECTION('center_axis',(0.,1.,0.));
#4092=DIRECTION('ref_axis',(1.,0.,0.));
#4093=DIRECTION('',(0.,-1.,0.));
#4094=DIRECTION('center_axis',(0.,1.,0.));
#4095=DIRECTION('ref_axis',(1.,0.,0.));
#4096=DIRECTION('center_axis',(0.,1.,0.));
#4097=DIRECTION('ref_axis',(1.,0.,0.));
#4098=DIRECTION('center_axis',(0.,1.,0.));
#4099=DIRECTION('ref_axis',(1.,0.,0.));
#4100=DIRECTION('axis',(0.,0.,1.));
#4101=DIRECTION('refdir',(1.,0.,0.));
#4102=DIRECTION('center_axis',(0.,1.,0.));
#4103=DIRECTION('ref_axis',(1.,0.,0.));
#4104=DIRECTION('center_axis',(0.,-1.,0.));
#4105=DIRECTION('ref_axis',(1.,0.,0.));
#4106=DIRECTION('',(0.,-1.,0.));
#4107=DIRECTION('center_axis',(0.,-1.,0.));
#4108=DIRECTION('ref_axis',(1.,0.,0.));
#4109=DIRECTION('center_axis',(0.,1.,0.));
#4110=DIRECTION('ref_axis',(1.,0.,0.));
#4111=DIRECTION('center_axis',(0.,1.,0.));
#4112=DIRECTION('ref_axis',(1.,0.,0.));
#4113=DIRECTION('',(0.,-1.,0.));
#4114=DIRECTION('center_axis',(0.,1.,0.));
#4115=DIRECTION('ref_axis',(1.,0.,0.));
#4116=DIRECTION('center_axis',(0.,1.,0.));
#4117=DIRECTION('ref_axis',(1.,0.,0.));
#4118=DIRECTION('center_axis',(0.,1.,0.));
#4119=DIRECTION('ref_axis',(1.,0.,0.));
#4120=DIRECTION('axis',(0.,0.,1.));
#4121=DIRECTION('refdir',(1.,0.,0.));
#4122=DIRECTION('center_axis',(0.,1.,0.));
#4123=DIRECTION('ref_axis',(1.,0.,0.));
#4124=DIRECTION('center_axis',(0.,-1.,0.));
#4125=DIRECTION('ref_axis',(1.,0.,0.));
#4126=DIRECTION('',(0.,-1.,0.));
#4127=DIRECTION('center_axis',(0.,-1.,0.));
#4128=DIRECTION('ref_axis',(1.,0.,0.));
#4129=DIRECTION('center_axis',(0.,1.,0.));
#4130=DIRECTION('ref_axis',(1.,0.,0.));
#4131=DIRECTION('center_axis',(0.,1.,0.));
#4132=DIRECTION('ref_axis',(1.,0.,0.));
#4133=DIRECTION('',(0.,-1.,0.));
#4134=DIRECTION('center_axis',(0.,1.,0.));
#4135=DIRECTION('ref_axis',(1.,0.,0.));
#4136=DIRECTION('center_axis',(0.,1.,0.));
#4137=DIRECTION('ref_axis',(1.,0.,0.));
#4138=DIRECTION('center_axis',(0.,1.,0.));
#4139=DIRECTION('ref_axis',(1.,0.,0.));
#4140=DIRECTION('axis',(0.,0.,1.));
#4141=DIRECTION('refdir',(1.,0.,0.));
#4142=DIRECTION('center_axis',(0.,1.,0.));
#4143=DIRECTION('ref_axis',(1.,0.,0.));
#4144=DIRECTION('center_axis',(0.,-1.,0.));
#4145=DIRECTION('ref_axis',(1.,0.,0.));
#4146=DIRECTION('',(0.,-1.,0.));
#4147=DIRECTION('center_axis',(0.,-1.,0.));
#4148=DIRECTION('ref_axis',(1.,0.,0.));
#4149=DIRECTION('center_axis',(0.,1.,0.));
#4150=DIRECTION('ref_axis',(1.,0.,0.));
#4151=DIRECTION('center_axis',(0.,1.,0.));
#4152=DIRECTION('ref_axis',(1.,0.,0.));
#4153=DIRECTION('',(0.,-1.,0.));
#4154=DIRECTION('center_axis',(0.,1.,0.));
#4155=DIRECTION('ref_axis',(1.,0.,0.));
#4156=DIRECTION('center_axis',(0.,1.,0.));
#4157=DIRECTION('ref_axis',(1.,0.,0.));
#4158=DIRECTION('center_axis',(0.,1.,0.));
#4159=DIRECTION('ref_axis',(1.,0.,0.));
#4160=DIRECTION('axis',(0.,0.,1.));
#4161=DIRECTION('refdir',(1.,0.,0.));
#4162=DIRECTION('center_axis',(0.,1.,0.));
#4163=DIRECTION('ref_axis',(1.,0.,0.));
#4164=DIRECTION('center_axis',(0.,-1.,0.));
#4165=DIRECTION('ref_axis',(1.,0.,0.));
#4166=DIRECTION('',(0.,-1.,0.));
#4167=DIRECTION('center_axis',(0.,-1.,0.));
#4168=DIRECTION('ref_axis',(1.,0.,0.));
#4169=DIRECTION('center_axis',(0.,1.,0.));
#4170=DIRECTION('ref_axis',(1.,0.,0.));
#4171=DIRECTION('center_axis',(0.,1.,0.));
#4172=DIRECTION('ref_axis',(1.,0.,0.));
#4173=DIRECTION('',(0.,-1.,0.));
#4174=DIRECTION('center_axis',(0.,1.,0.));
#4175=DIRECTION('ref_axis',(1.,0.,0.));
#4176=DIRECTION('center_axis',(0.,1.,0.));
#4177=DIRECTION('ref_axis',(1.,0.,0.));
#4178=DIRECTION('center_axis',(0.,1.,0.));
#4179=DIRECTION('ref_axis',(1.,0.,0.));
#4180=DIRECTION('axis',(0.,0.,1.));
#4181=DIRECTION('refdir',(1.,0.,0.));
#4182=DIRECTION('center_axis',(0.,1.,0.));
#4183=DIRECTION('ref_axis',(1.,0.,0.));
#4184=DIRECTION('center_axis',(0.,-1.,0.));
#4185=DIRECTION('ref_axis',(1.,0.,0.));
#4186=DIRECTION('',(0.,-1.,0.));
#4187=DIRECTION('center_axis',(0.,-1.,0.));
#4188=DIRECTION('ref_axis',(1.,0.,0.));
#4189=DIRECTION('center_axis',(0.,1.,0.));
#4190=DIRECTION('ref_axis',(1.,0.,0.));
#4191=DIRECTION('center_axis',(0.,1.,0.));
#4192=DIRECTION('ref_axis',(1.,0.,0.));
#4193=DIRECTION('',(0.,-1.,0.));
#4194=DIRECTION('center_axis',(0.,1.,0.));
#4195=DIRECTION('ref_axis',(1.,0.,0.));
#4196=DIRECTION('center_axis',(0.,1.,0.));
#4197=DIRECTION('ref_axis',(1.,0.,0.));
#4198=DIRECTION('center_axis',(0.,1.,0.));
#4199=DIRECTION('ref_axis',(1.,0.,0.));
#4200=DIRECTION('axis',(0.,0.,1.));
#4201=DIRECTION('refdir',(1.,0.,0.));
#4202=DIRECTION('center_axis',(0.,1.,0.));
#4203=DIRECTION('ref_axis',(1.,0.,0.));
#4204=DIRECTION('center_axis',(0.,-1.,0.));
#4205=DIRECTION('ref_axis',(1.,0.,0.));
#4206=DIRECTION('',(0.,-1.,0.));
#4207=DIRECTION('center_axis',(0.,-1.,0.));
#4208=DIRECTION('ref_axis',(1.,0.,0.));
#4209=DIRECTION('center_axis',(0.,1.,0.));
#4210=DIRECTION('ref_axis',(1.,0.,0.));
#4211=DIRECTION('center_axis',(0.,1.,0.));
#4212=DIRECTION('ref_axis',(1.,0.,0.));
#4213=DIRECTION('',(0.,-1.,0.));
#4214=DIRECTION('center_axis',(0.,1.,0.));
#4215=DIRECTION('ref_axis',(1.,0.,0.));
#4216=DIRECTION('center_axis',(0.,1.,0.));
#4217=DIRECTION('ref_axis',(1.,0.,0.));
#4218=DIRECTION('center_axis',(0.,1.,0.));
#4219=DIRECTION('ref_axis',(1.,0.,0.));
#4220=DIRECTION('axis',(0.,0.,1.));
#4221=DIRECTION('refdir',(1.,0.,0.));
#4222=DIRECTION('center_axis',(0.,1.,0.));
#4223=DIRECTION('ref_axis',(1.,0.,0.));
#4224=DIRECTION('center_axis',(0.,-1.,0.));
#4225=DIRECTION('ref_axis',(1.,0.,0.));
#4226=DIRECTION('',(0.,-1.,0.));
#4227=DIRECTION('center_axis',(0.,-1.,0.));
#4228=DIRECTION('ref_axis',(1.,0.,0.));
#4229=DIRECTION('center_axis',(0.,1.,0.));
#4230=DIRECTION('ref_axis',(1.,0.,0.));
#4231=DIRECTION('center_axis',(0.,1.,0.));
#4232=DIRECTION('ref_axis',(1.,0.,0.));
#4233=DIRECTION('',(0.,-1.,0.));
#4234=DIRECTION('center_axis',(0.,1.,0.));
#4235=DIRECTION('ref_axis',(1.,0.,0.));
#4236=DIRECTION('center_axis',(0.,1.,0.));
#4237=DIRECTION('ref_axis',(1.,0.,0.));
#4238=DIRECTION('center_axis',(0.,1.,0.));
#4239=DIRECTION('ref_axis',(1.,0.,0.));
#4240=DIRECTION('axis',(0.,0.,1.));
#4241=DIRECTION('refdir',(1.,0.,0.));
#4242=DIRECTION('axis',(0.,0.,1.));
#4243=DIRECTION('refdir',(1.,0.,0.));
#4244=DIRECTION('center_axis',(0.,1.,0.));
#4245=DIRECTION('ref_axis',(1.,0.,0.));
#4246=DIRECTION('center_axis',(0.,1.,0.));
#4247=DIRECTION('ref_axis',(1.,0.,0.));
#4248=DIRECTION('',(0.,1.,0.));
#4249=DIRECTION('center_axis',(0.,-1.,0.));
#4250=DIRECTION('ref_axis',(1.,0.,0.));
#4251=DIRECTION('center_axis',(0.,1.,0.));
#4252=DIRECTION('ref_axis',(1.,0.,0.));
#4253=DIRECTION('center_axis',(0.,1.,0.));
#4254=DIRECTION('ref_axis',(1.,0.,0.));
#4255=DIRECTION('',(0.,1.,0.));
#4256=DIRECTION('center_axis',(0.,-1.,0.));
#4257=DIRECTION('ref_axis',(1.,0.,0.));
#4258=DIRECTION('center_axis',(6.12323399573677E-17,0.,1.));
#4259=DIRECTION('ref_axis',(1.,0.,0.));
#4260=DIRECTION('center_axis',(-1.22464679914735E-16,1.,0.));
#4261=DIRECTION('ref_axis',(-1.,-1.22464679914735E-16,0.));
#4262=DIRECTION('center_axis',(0.,1.,0.));
#4263=DIRECTION('ref_axis',(1.,0.,0.));
#4264=DIRECTION('center_axis',(0.,1.,0.));
#4265=DIRECTION('ref_axis',(1.,0.,0.));
#4266=DIRECTION('',(0.,-1.,0.));
#4267=DIRECTION('center_axis',(0.,-1.,0.));
#4268=DIRECTION('ref_axis',(1.,0.,0.));
#4269=DIRECTION('center_axis',(0.,1.,0.));
#4270=DIRECTION('ref_axis',(1.,0.,0.));
#4271=DIRECTION('center_axis',(0.,1.,0.));
#4272=DIRECTION('ref_axis',(1.,0.,0.));
#4273=DIRECTION('',(0.,-1.,0.));
#4274=DIRECTION('center_axis',(0.,-1.,0.));
#4275=DIRECTION('ref_axis',(1.,0.,0.));
#4276=DIRECTION('center_axis',(0.,1.,0.));
#4277=DIRECTION('ref_axis',(1.,0.,0.));
#4278=DIRECTION('center_axis',(0.,1.,0.));
#4279=DIRECTION('ref_axis',(1.,0.,0.));
#4280=DIRECTION('center_axis',(0.,1.,0.));
#4281=DIRECTION('ref_axis',(1.,0.,0.));
#4282=DIRECTION('center_axis',(0.,1.,0.));
#4283=DIRECTION('ref_axis',(1.,0.,0.));
#4284=DIRECTION('',(0.,1.,0.));
#4285=DIRECTION('center_axis',(0.,-1.,0.));
#4286=DIRECTION('ref_axis',(1.,0.,0.));
#4287=DIRECTION('center_axis',(0.,1.,0.));
#4288=DIRECTION('ref_axis',(1.,0.,0.));
#4289=DIRECTION('center_axis',(0.,1.,0.));
#4290=DIRECTION('ref_axis',(1.,0.,0.));
#4291=DIRECTION('',(0.,1.,0.));
#4292=DIRECTION('center_axis',(0.,-1.,0.));
#4293=DIRECTION('ref_axis',(1.,0.,0.));
#4294=DIRECTION('center_axis',(0.,1.,0.));
#4295=DIRECTION('ref_axis',(1.,0.,0.));
#4296=DIRECTION('center_axis',(0.,1.,0.));
#4297=DIRECTION('ref_axis',(1.,0.,0.));
#4298=DIRECTION('',(0.,1.,0.));
#4299=DIRECTION('center_axis',(0.,-1.,0.));
#4300=DIRECTION('ref_axis',(1.,0.,0.));
#4301=DIRECTION('center_axis',(0.,1.,0.));
#4302=DIRECTION('ref_axis',(1.,0.,0.));
#4303=DIRECTION('center_axis',(0.,1.,0.));
#4304=DIRECTION('ref_axis',(1.,0.,0.));
#4305=DIRECTION('',(0.,1.,0.));
#4306=DIRECTION('center_axis',(0.,-1.,0.));
#4307=DIRECTION('ref_axis',(1.,0.,0.));
#4308=DIRECTION('center_axis',(-1.,0.,0.));
#4309=DIRECTION('ref_axis',(0.,0.,1.));
#4310=DIRECTION('',(0.,0.,1.));
#4311=DIRECTION('',(0.,1.,0.));
#4312=DIRECTION('',(0.,0.,1.));
#4313=DIRECTION('',(0.,1.,0.));
#4314=DIRECTION('center_axis',(-0.707106781186548,0.,-0.707106781186548));
#4315=DIRECTION('ref_axis',(-0.707106781186548,0.,0.707106781186548));
#4316=DIRECTION('',(-0.707106781186548,0.,0.707106781186548));
#4317=DIRECTION('',(-0.707106781186548,0.,0.707106781186548));
#4318=DIRECTION('',(0.,1.,0.));
#4319=DIRECTION('center_axis',(0.,0.,-1.));
#4320=DIRECTION('ref_axis',(-1.,0.,0.));
#4321=DIRECTION('',(-1.,0.,0.));
#4322=DIRECTION('',(-1.,0.,0.));
#4323=DIRECTION('',(0.,1.,0.));
#4324=DIRECTION('center_axis',(0.707106781186548,0.,-0.707106781186548));
#4325=DIRECTION('ref_axis',(-0.707106781186548,0.,-0.707106781186548));
#4326=DIRECTION('',(-0.707106781186548,0.,-0.707106781186548));
#4327=DIRECTION('',(-0.707106781186548,0.,-0.707106781186548));
#4328=DIRECTION('',(0.,1.,0.));
#4329=DIRECTION('center_axis',(1.,0.,0.));
#4330=DIRECTION('ref_axis',(0.,0.,-1.));
#4331=DIRECTION('',(0.,0.,-1.));
#4332=DIRECTION('',(0.,0.,-1.));
#4333=DIRECTION('',(0.,1.,0.));
#4334=DIRECTION('center_axis',(0.707106781186548,0.,0.707106781186548));
#4335=DIRECTION('ref_axis',(0.707106781186548,0.,-0.707106781186548));
#4336=DIRECTION('',(0.707106781186548,0.,-0.707106781186548));
#4337=DIRECTION('',(0.707106781186548,0.,-0.707106781186548));
#4338=DIRECTION('',(0.,1.,0.));
#4339=DIRECTION('center_axis',(0.,0.,1.));
#4340=DIRECTION('ref_axis',(1.,0.,0.));
#4341=DIRECTION('',(1.,0.,0.));
#4342=DIRECTION('',(1.,0.,0.));
#4343=DIRECTION('',(0.,1.,0.));
#4344=DIRECTION('center_axis',(-0.707106781186548,0.,0.707106781186548));
#4345=DIRECTION('ref_axis',(0.707106781186548,0.,0.707106781186548));
#4346=DIRECTION('',(0.707106781186548,0.,0.707106781186548));
#4347=DIRECTION('',(0.707106781186548,0.,0.707106781186548));
#4348=DIRECTION('center_axis',(0.,1.,0.));
#4349=DIRECTION('ref_axis',(0.,0.,1.));
#4350=DIRECTION('center_axis',(0.,1.,0.));
#4351=DIRECTION('ref_axis',(1.,0.,0.));
#4352=DIRECTION('axis',(0.,0.,1.));
#4353=DIRECTION('refdir',(1.,0.,0.));
#4354=DIRECTION('center_axis',(0.,-1.,0.));
#4355=DIRECTION('ref_axis',(1.,0.,0.));
#4356=DIRECTION('center_axis',(0.,-1.,0.));
#4357=DIRECTION('ref_axis',(1.,0.,0.));
#4358=DIRECTION('',(0.,1.,0.));
#4359=DIRECTION('center_axis',(0.,-1.,0.));
#4360=DIRECTION('ref_axis',(1.,0.,0.));
#4361=DIRECTION('center_axis',(0.,1.,0.));
#4362=DIRECTION('ref_axis',(0.,0.,1.));
#4363=DIRECTION('center_axis',(0.,-1.,0.));
#4364=DIRECTION('ref_axis',(1.,0.,0.));
#4365=DIRECTION('center_axis',(6.12323399573677E-17,0.,1.));
#4366=DIRECTION('ref_axis',(1.,0.,0.));
#4367=DIRECTION('center_axis',(1.22464679914735E-16,-1.,0.));
#4368=DIRECTION('ref_axis',(-1.,-1.22464679914735E-16,0.));
#4369=DIRECTION('center_axis',(0.,-1.,0.));
#4370=DIRECTION('ref_axis',(1.,0.,0.));
#4371=DIRECTION('center_axis',(0.,-1.,0.));
#4372=DIRECTION('ref_axis',(0.,0.,-1.));
#4373=DIRECTION('center_axis',(-0.866025403784438,0.,-0.5));
#4374=DIRECTION('ref_axis',(-0.5,0.,0.866025403784438));
#4375=DIRECTION('',(-0.866025403784438,0.,-0.5));
#4376=DIRECTION('center_axis',(-0.866025403784438,0.,-0.5));
#4377=DIRECTION('ref_axis',(-0.5,0.,0.866025403784438));
#4378=DIRECTION('',(-0.866025403784438,0.,-0.5));
#4379=DIRECTION('center_axis',(0.,-1.,0.));
#4380=DIRECTION('ref_axis',(1.,0.,0.));
#4381=DIRECTION('center_axis',(0.,-1.,0.));
#4382=DIRECTION('ref_axis',(1.,0.,0.));
#4383=DIRECTION('',(0.,1.,0.));
#4384=DIRECTION('center_axis',(0.,-1.,0.));
#4385=DIRECTION('ref_axis',(1.,0.,0.));
#4386=DIRECTION('center_axis',(0.866025403784439,0.,-0.5));
#4387=DIRECTION('ref_axis',(-0.5,0.,-0.866025403784439));
#4388=DIRECTION('',(0.866025403784439,0.,-0.5));
#4389=DIRECTION('center_axis',(0.866025403784439,0.,-0.5));
#4390=DIRECTION('ref_axis',(-0.5,0.,-0.866025403784439));
#4391=DIRECTION('',(0.866025403784439,0.,-0.5));
#4392=DIRECTION('center_axis',(0.,0.,1.));
#4393=DIRECTION('ref_axis',(1.,0.,0.));
#4394=DIRECTION('',(0.,0.,1.));
#4395=DIRECTION('center_axis',(0.,0.,1.));
#4396=DIRECTION('ref_axis',(1.,0.,0.));
#4397=DIRECTION('',(0.,0.,1.));
#4398=DIRECTION('center_axis',(0.,1.,0.));
#4399=DIRECTION('ref_axis',(0.,0.,1.));
#4400=DIRECTION('center_axis',(0.,-1.,0.));
#4401=DIRECTION('ref_axis',(1.,0.,0.));
#4402=DIRECTION('center_axis',(0.,1.,0.));
#4403=DIRECTION('ref_axis',(0.,0.,1.));
#4404=DIRECTION('center_axis',(0.,-1.,0.));
#4405=DIRECTION('ref_axis',(1.,0.,0.));
#4406=DIRECTION('center_axis',(0.,-1.,0.));
#4407=DIRECTION('ref_axis',(1.,0.,0.));
#4408=DIRECTION('center_axis',(0.,-1.,0.));
#4409=DIRECTION('ref_axis',(1.,0.,0.));
#4410=DIRECTION('',(0.,1.,0.));
#4411=DIRECTION('center_axis',(0.,-1.,0.));
#4412=DIRECTION('ref_axis',(0.,0.,-1.));
#4413=DIRECTION('center_axis',(0.,-1.,0.));
#4414=DIRECTION('ref_axis',(1.,0.,0.));
#4415=DIRECTION('center_axis',(0.,-1.,0.));
#4416=DIRECTION('ref_axis',(1.,0.,0.));
#4417=DIRECTION('',(0.,1.,0.));
#4418=DIRECTION('',(0.,0.,1.));
#4419=DIRECTION('',(1.,0.,0.));
#4420=DIRECTION('',(0.,0.,1.));
#4421=DIRECTION('',(1.,0.,0.));
#4422=DIRECTION('axis',(0.,0.,1.));
#4423=DIRECTION('refdir',(1.,0.,0.));
#4424=DIRECTION('center_axis',(0.,1.,0.));
#4425=DIRECTION('ref_axis',(1.,0.,0.));
#4426=DIRECTION('center_axis',(0.,-1.,0.));
#4427=DIRECTION('ref_axis',(1.,0.,0.));
#4428=DIRECTION('',(0.,-1.,0.));
#4429=DIRECTION('center_axis',(0.,-1.,0.));
#4430=DIRECTION('ref_axis',(1.,0.,0.));
#4431=DIRECTION('center_axis',(0.,1.,0.));
#4432=DIRECTION('ref_axis',(1.,0.,0.));
#4433=DIRECTION('center_axis',(0.,1.,0.));
#4434=DIRECTION('ref_axis',(1.,0.,0.));
#4435=DIRECTION('',(0.,-1.,0.));
#4436=DIRECTION('center_axis',(0.,1.,0.));
#4437=DIRECTION('ref_axis',(1.,0.,0.));
#4438=DIRECTION('center_axis',(0.,1.,0.));
#4439=DIRECTION('ref_axis',(1.,0.,0.));
#4440=DIRECTION('center_axis',(0.,1.,0.));
#4441=DIRECTION('ref_axis',(1.,0.,0.));
#4442=DIRECTION('axis',(0.,0.,1.));
#4443=DIRECTION('refdir',(1.,0.,0.));
#4444=DIRECTION('center_axis',(0.,1.,0.));
#4445=DIRECTION('ref_axis',(0.,0.,1.));
#4446=DIRECTION('center_axis',(0.,-1.,0.));
#4447=DIRECTION('ref_axis',(1.,0.,0.));
#4448=DIRECTION('center_axis',(0.,-1.,0.));
#4449=DIRECTION('ref_axis',(1.,0.,0.));
#4450=DIRECTION('center_axis',(0.,-1.,0.));
#4451=DIRECTION('ref_axis',(1.,0.,0.));
#4452=DIRECTION('',(0.707106781186548,0.707106781186547,8.65956056235493E-17));
#4453=DIRECTION('center_axis',(0.,-1.,0.));
#4454=DIRECTION('ref_axis',(1.,0.,0.));
#4455=DIRECTION('center_axis',(0.,-1.,0.));
#4456=DIRECTION('ref_axis',(1.,0.,0.));
#4457=DIRECTION('',(0.,1.,0.));
#4458=DIRECTION('center_axis',(0.,1.,0.));
#4459=DIRECTION('ref_axis',(1.,0.,0.));
#4460=DIRECTION('center_axis',(0.,-1.,0.));
#4461=DIRECTION('ref_axis',(1.,0.,0.));
#4462=DIRECTION('',(-0.707106781186548,0.707106781186547,-8.65956056235494E-17));
#4463=DIRECTION('center_axis',(0.,-1.,0.));
#4464=DIRECTION('ref_axis',(0.,0.,-1.));
#4465=DIRECTION('center_axis',(0.,-1.,0.));
#4466=DIRECTION('ref_axis',(1.,0.,0.));
#4467=DIRECTION('center_axis',(0.,1.,0.));
#4468=DIRECTION('ref_axis',(1.,0.,0.));
#4469=DIRECTION('center_axis',(0.,1.,0.));
#4470=DIRECTION('ref_axis',(1.,0.,0.));
#4471=DIRECTION('',(-0.447213595499958,0.894427190999916,-5.47678698264203E-17));
#4472=DIRECTION('center_axis',(0.,-1.,0.));
#4473=DIRECTION('ref_axis',(1.,0.,0.));
#4474=DIRECTION('center_axis',(0.,1.,0.));
#4475=DIRECTION('ref_axis',(1.,0.,0.));
#4476=DIRECTION('',(0.,1.,0.));
#4477=DIRECTION('center_axis',(0.,1.,0.));
#4478=DIRECTION('ref_axis',(1.,0.,0.));
#4479=DIRECTION('center_axis',(0.,-1.,0.));
#4480=DIRECTION('ref_axis',(1.,0.,0.));
#4481=DIRECTION('',(-0.707106781186547,0.707106781186548,-8.65956056235493E-17));
#4482=DIRECTION('center_axis',(0.,-1.,0.));
#4483=DIRECTION('ref_axis',(0.,0.,-1.));
#4484=DIRECTION('center_axis',(0.866025403784439,0.,-0.5));
#4485=DIRECTION('ref_axis',(0.5,0.,0.866025403784439));
#4486=DIRECTION('',(-0.5,0.,-0.866025403784439));
#4487=DIRECTION('',(0.,-1.,0.));
#4488=DIRECTION('',(0.5,0.,0.866025403784439));
#4489=DIRECTION('',(0.,-1.,0.));
#4490=DIRECTION('center_axis',(1.60246890531964E-16,0.,-1.));
#4491=DIRECTION('ref_axis',(1.,0.,1.60246890531964E-16));
#4492=DIRECTION('',(-1.,0.,-1.60246890531964E-16));
#4493=DIRECTION('',(0.,-1.,0.));
#4494=DIRECTION('',(1.,0.,1.60246890531964E-16));
#4495=DIRECTION('center_axis',(-0.866025403784439,0.,-0.5));
#4496=DIRECTION('ref_axis',(0.5,0.,-0.866025403784439));
#4497=DIRECTION('',(-0.5,0.,0.866025403784439));
#4498=DIRECTION('',(0.,-1.,0.));
#4499=DIRECTION('',(0.5,0.,-0.866025403784439));
#4500=DIRECTION('center_axis',(-0.866025403784439,0.,0.5));
#4501=DIRECTION('ref_axis',(-0.5,0.,-0.866025403784439));
#4502=DIRECTION('',(0.5,0.,0.866025403784439));
#4503=DIRECTION('',(0.,-1.,0.));
#4504=DIRECTION('',(-0.5,0.,-0.866025403784439));
#4505=DIRECTION('center_axis',(-1.60246890531964E-16,0.,1.));
#4506=DIRECTION('ref_axis',(-1.,0.,-1.60246890531964E-16));
#4507=DIRECTION('',(1.,0.,1.60246890531964E-16));
#4508=DIRECTION('',(0.,-1.,0.));
#4509=DIRECTION('',(-1.,0.,-1.60246890531964E-16));
#4510=DIRECTION('center_axis',(0.866025403784439,0.,0.5));
#4511=DIRECTION('ref_axis',(-0.5,0.,0.866025403784439));
#4512=DIRECTION('',(0.5,0.,-0.866025403784439));
#4513=DIRECTION('',(-0.5,0.,0.866025403784439));
#4514=DIRECTION('center_axis',(0.,1.,0.));
#4515=DIRECTION('ref_axis',(1.,0.,0.));
#4516=DIRECTION('center_axis',(0.,-1.,0.));
#4517=DIRECTION('ref_axis',(0.,0.,-1.));
#4518=DIRECTION('',(0.,0.,1.));
#4519=DIRECTION('',(1.,0.,0.));
#4520=DIRECTION('',(0.,0.,1.));
#4521=DIRECTION('',(1.,0.,0.));
#4522=DIRECTION('',(0.,0.,1.));
#4523=DIRECTION('',(1.,0.,0.));
#4524=DIRECTION('',(0.,0.,1.));
#4525=DIRECTION('',(1.,0.,0.));
#4526=DIRECTION('',(0.,0.,1.));
#4527=DIRECTION('',(1.,0.,0.));
#4528=DIRECTION('',(0.,0.,1.));
#4529=DIRECTION('',(1.,0.,0.));
#4530=DIRECTION('',(0.,0.,1.));
#4531=DIRECTION('',(1.,0.,0.));
#4532=DIRECTION('',(0.,0.,1.));
#4533=DIRECTION('',(1.,0.,0.));
#4534=DIRECTION('',(0.,0.,1.));
#4535=DIRECTION('',(1.,0.,0.));
#4536=DIRECTION('',(0.,0.,1.));
#4537=DIRECTION('',(1.,0.,0.));
#4538=DIRECTION('',(0.,0.,1.));
#4539=DIRECTION('',(-1.,1.22464679914735E-16,0.));
#4540=DIRECTION('',(0.,0.,1.));
#4541=DIRECTION('',(-1.,1.22464679914735E-16,0.));
#4542=DIRECTION('',(0.,0.,1.));
#4543=DIRECTION('',(-1.,1.22464679914735E-16,0.));
#4544=DIRECTION('',(0.,0.,1.));
#4545=DIRECTION('',(-1.,1.22464679914735E-16,0.));
#4546=DIRECTION('',(0.,0.,1.));
#4547=DIRECTION('',(-1.,1.22464679914735E-16,0.));
#4548=DIRECTION('',(0.,0.,1.));
#4549=DIRECTION('',(-1.,1.22464679914735E-16,0.));
#4550=DIRECTION('',(0.,0.,1.));
#4551=DIRECTION('',(-1.,1.22464679914735E-16,0.));
#4552=DIRECTION('',(0.,0.,1.));
#4553=DIRECTION('',(-1.,1.22464679914735E-16,0.));
#4554=DIRECTION('',(0.,0.,1.));
#4555=DIRECTION('',(1.,0.,0.));
#4556=DIRECTION('',(0.,0.,1.));
#4557=DIRECTION('',(1.,0.,0.));
#4558=DIRECTION('',(0.,0.,1.));
#4559=DIRECTION('',(1.,0.,0.));
#4560=DIRECTION('',(0.,0.,1.));
#4561=DIRECTION('',(1.,0.,0.));
#4562=DIRECTION('',(0.,0.,1.));
#4563=DIRECTION('',(1.,0.,0.));
#4564=DIRECTION('',(0.,0.,1.));
#4565=DIRECTION('',(1.,0.,0.));
#4566=DIRECTION('',(0.,0.,1.));
#4567=DIRECTION('',(1.,0.,0.));
#4568=DIRECTION('',(0.,0.,1.));
#4569=DIRECTION('',(1.,0.,0.));
#4570=DIRECTION('',(0.,0.,1.));
#4571=DIRECTION('',(1.,0.,0.));
#4572=DIRECTION('axis',(0.,0.,1.));
#4573=DIRECTION('refdir',(1.,0.,0.));
#4574=DIRECTION('axis',(0.,0.,1.));
#4575=DIRECTION('refdir',(1.,0.,0.));
#4576=DIRECTION('center_axis',(-1.,0.,0.));
#4577=DIRECTION('ref_axis',(0.,0.,1.));
#4578=DIRECTION('',(0.,1.,0.));
#4579=DIRECTION('',(0.,0.,-1.));
#4580=DIRECTION('',(0.,1.,0.));
#4581=DIRECTION('',(0.,0.,1.));
#4582=DIRECTION('center_axis',(0.,1.,0.));
#4583=DIRECTION('ref_axis',(0.,0.,1.));
#4584=DIRECTION('center_axis',(0.,1.,0.));
#4585=DIRECTION('ref_axis',(1.,0.,0.));
#4586=DIRECTION('',(-1.,0.,0.));
#4587=DIRECTION('',(0.,0.,-1.));
#4588=DIRECTION('center_axis',(0.,0.,-1.));
#4589=DIRECTION('ref_axis',(-1.,0.,0.));
#4590=DIRECTION('',(1.,0.,0.));
#4591=DIRECTION('',(0.,1.,0.));
#4592=DIRECTION('center_axis',(1.,0.,0.));
#4593=DIRECTION('ref_axis',(0.,0.,-1.));
#4594=DIRECTION('',(0.,-1.,0.));
#4595=DIRECTION('',(0.,0.,1.));
#4596=DIRECTION('center_axis',(0.,1.,0.));
#4597=DIRECTION('ref_axis',(1.,0.,0.));
#4598=DIRECTION('center_axis',(0.,-1.,0.));
#4599=DIRECTION('ref_axis',(1.,0.,0.));
#4600=DIRECTION('center_axis',(0.,1.,0.));
#4601=DIRECTION('ref_axis',(1.,0.,0.));
#4602=DIRECTION('center_axis',(0.,1.,0.));
#4603=DIRECTION('ref_axis',(1.,0.,0.));
#4604=DIRECTION('',(0.,-1.,0.));
#4605=DIRECTION('center_axis',(0.,1.,0.));
#4606=DIRECTION('ref_axis',(1.,0.,0.));
#4607=DIRECTION('center_axis',(0.,1.,0.));
#4608=DIRECTION('ref_axis',(1.,0.,0.));
#4609=DIRECTION('center_axis',(0.,1.,0.));
#4610=DIRECTION('ref_axis',(1.,0.,0.));
#4611=DIRECTION('axis',(0.,0.,1.));
#4612=DIRECTION('refdir',(1.,0.,0.));
#4613=DIRECTION('axis',(0.,0.,1.));
#4614=DIRECTION('refdir',(1.,0.,0.));
#4615=DIRECTION('center_axis',(0.,1.,0.));
#4616=DIRECTION('ref_axis',(0.,0.,1.));
#4617=DIRECTION('center_axis',(0.,-1.,0.));
#4618=DIRECTION('ref_axis',(1.,0.,0.));
#4619=DIRECTION('center_axis',(0.,-1.,0.));
#4620=DIRECTION('ref_axis',(1.,0.,0.));
#4621=DIRECTION('center_axis',(0.,-1.,0.));
#4622=DIRECTION('ref_axis',(1.,0.,0.));
#4623=DIRECTION('',(0.371390676354104,0.928476690885259,4.54822403030224E-17));
#4624=DIRECTION('center_axis',(0.,-1.,0.));
#4625=DIRECTION('ref_axis',(1.,0.,0.));
#4626=DIRECTION('center_axis',(0.,-1.,0.));
#4627=DIRECTION('ref_axis',(1.,0.,0.));
#4628=DIRECTION('',(0.,1.,0.));
#4629=DIRECTION('center_axis',(0.,-1.,0.));
#4630=DIRECTION('ref_axis',(0.,0.,-1.));
#4631=DIRECTION('center_axis',(0.,-1.,0.));
#4632=DIRECTION('ref_axis',(1.,0.,0.));
#4633=DIRECTION('center_axis',(0.,-1.,0.));
#4634=DIRECTION('ref_axis',(1.,0.,0.));
#4635=DIRECTION('center_axis',(0.,-1.,0.));
#4636=DIRECTION('ref_axis',(1.,0.,0.));
#4637=DIRECTION('',(0.,1.,0.));
#4638=DIRECTION('center_axis',(0.,-1.,0.));
#4639=DIRECTION('ref_axis',(0.,0.,-1.));
#4640=DIRECTION('center_axis',(0.,1.,0.));
#4641=DIRECTION('ref_axis',(1.,0.,0.));
#4642=DIRECTION('',(0.,1.,0.));
#4643=DIRECTION('center_axis',(-1.,0.,0.));
#4644=DIRECTION('ref_axis',(0.,0.,-1.));
#4645=DIRECTION('',(-1.,0.,0.));
#4646=DIRECTION('center_axis',(-1.,0.,0.));
#4647=DIRECTION('ref_axis',(0.,0.,1.));
#4648=DIRECTION('',(0.,0.,-1.));
#4649=DIRECTION('',(0.,-1.,0.));
#4650=DIRECTION('',(0.,0.,1.));
#4651=DIRECTION('',(0.,-1.,0.));
#4652=DIRECTION('center_axis',(1.,0.,0.));
#4653=DIRECTION('ref_axis',(0.,0.,-1.));
#4654=DIRECTION('',(0.,0.,1.));
#4655=DIRECTION('',(0.,1.,0.));
#4656=DIRECTION('',(0.,0.,-1.));
#4657=DIRECTION('',(0.,1.,0.));
#4658=DIRECTION('center_axis',(0.,0.,1.));
#4659=DIRECTION('ref_axis',(1.,0.,0.));
#4660=DIRECTION('',(-1.,0.,0.));
#4661=DIRECTION('',(1.,0.,0.));
#4662=DIRECTION('center_axis',(0.,-1.,0.));
#4663=DIRECTION('ref_axis',(0.,0.,-1.));
#4664=DIRECTION('center_axis',(0.,-1.,0.));
#4665=DIRECTION('ref_axis',(1.,0.,0.));
#4666=DIRECTION('center_axis',(0.,-1.,0.));
#4667=DIRECTION('ref_axis',(1.,0.,0.));
#4668=DIRECTION('center_axis',(0.,-1.,0.));
#4669=DIRECTION('ref_axis',(-1.83697019872103E-16,0.,-1.));
#4670=DIRECTION('center_axis',(0.,-1.,0.));
#4671=DIRECTION('ref_axis',(1.,0.,0.));
#4672=DIRECTION('center_axis',(-0.5,0.,0.866025403784438));
#4673=DIRECTION('ref_axis',(0.866025403784438,0.,0.5));
#4674=DIRECTION('',(0.5,0.,-0.866025403784438));
#4675=DIRECTION('center_axis',(-0.5,0.,-0.866025403784439));
#4676=DIRECTION('ref_axis',(-0.866025403784439,0.,0.5));
#4677=DIRECTION('',(0.5,0.,0.866025403784439));
#4678=DIRECTION('center_axis',(1.,0.,0.));
#4679=DIRECTION('ref_axis',(0.,0.,-1.));
#4680=DIRECTION('',(-1.,0.,0.));
#4681=DIRECTION('center_axis',(0.,1.,0.));
#4682=DIRECTION('ref_axis',(0.,0.,1.));
#4683=DIRECTION('center_axis',(0.,-1.,0.));
#4684=DIRECTION('ref_axis',(1.,0.,0.));
#4685=DIRECTION('center_axis',(0.,-1.,0.));
#4686=DIRECTION('ref_axis',(1.,0.,0.));
#4687=DIRECTION('',(0.,1.,0.));
#4688=DIRECTION('',(0.,1.,0.));
#4689=DIRECTION('center_axis',(0.,-1.,0.));
#4690=DIRECTION('ref_axis',(0.,0.,-1.));
#4691=DIRECTION('center_axis',(-1.,0.,-1.22464679914735E-16));
#4692=DIRECTION('ref_axis',(-1.22464679914735E-16,0.,1.));
#4693=DIRECTION('center_axis',(0.,1.,0.));
#4694=DIRECTION('ref_axis',(0.,0.,-1.));
#4695=DIRECTION('center_axis',(0.,1.,0.));
#4696=DIRECTION('ref_axis',(0.,0.,-1.));
#4697=DIRECTION('center_axis',(0.,1.,0.));
#4698=DIRECTION('ref_axis',(0.,0.,-1.));
#4699=DIRECTION('center_axis',(0.,1.,0.));
#4700=DIRECTION('ref_axis',(0.,0.,-1.));
#4701=DIRECTION('',(0.,0.,1.));
#4702=DIRECTION('',(1.,0.,0.));
#4703=DIRECTION('axis',(0.,0.,1.));
#4704=DIRECTION('refdir',(1.,0.,0.));
#4705=DIRECTION('center_axis',(0.,0.707106781186548,0.707106781186547));
#4706=DIRECTION('ref_axis',(1.,0.,0.));
#4707=DIRECTION('',(-1.96261557335472E-15,-0.707106781186547,0.707106781186548));
#4708=DIRECTION('',(1.,0.,0.));
#4709=DIRECTION('',(0.,0.707106781186547,-0.707106781186548));
#4710=DIRECTION('',(-1.,0.,0.));
#4711=DIRECTION('center_axis',(0.,0.,-1.));
#4712=DIRECTION('ref_axis',(0.,1.,0.));
#4713=DIRECTION('',(0.,0.707106781186548,0.707106781186548));
#4714=DIRECTION('center_axis',(0.,0.,-1.));
#4715=DIRECTION('ref_axis',(0.,1.,0.));
#4716=DIRECTION('center_axis',(0.,0.,1.));
#4717=DIRECTION('ref_axis',(0.,1.,0.));
#4718=DIRECTION('center_axis',(0.,-0.707106781186548,0.707106781186547));
#4719=DIRECTION('ref_axis',(1.,0.,0.));
#4720=DIRECTION('',(1.96261557335472E-15,0.707106781186547,0.707106781186548));
#4721=DIRECTION('',(-1.,0.,0.));
#4722=DIRECTION('',(1.,0.,0.));
#4723=DIRECTION('center_axis',(0.,0.,-1.));
#4724=DIRECTION('ref_axis',(0.,-1.,0.));
#4725=DIRECTION('center_axis',(0.,0.,-1.));
#4726=DIRECTION('ref_axis',(0.,-1.,0.));
#4727=DIRECTION('center_axis',(0.,0.,1.));
#4728=DIRECTION('ref_axis',(0.,-1.,0.));
#4729=DIRECTION('center_axis',(0.,0.,1.));
#4730=DIRECTION('ref_axis',(0.,1.,0.));
#4731=DIRECTION('',(0.,0.,1.));
#4732=DIRECTION('center_axis',(0.,0.,-1.));
#4733=DIRECTION('ref_axis',(0.,1.,0.));
#4734=DIRECTION('',(0.,0.,1.));
#4735=DIRECTION('center_axis',(0.,1.,0.));
#4736=DIRECTION('ref_axis',(-1.,0.,0.));
#4737=DIRECTION('',(0.,0.,1.));
#4738=DIRECTION('',(1.,0.,0.));
#4739=DIRECTION('center_axis',(0.,0.,1.));
#4740=DIRECTION('ref_axis',(1.,0.,0.));
#4741=DIRECTION('center_axis',(0.,0.707106781186548,-0.707106781186548));
#4742=DIRECTION('ref_axis',(-1.,0.,0.));
#4743=DIRECTION('',(1.96261557335472E-15,0.707106781186548,0.707106781186548));
#4744=DIRECTION('',(0.,-0.707106781186548,-0.707106781186548));
#4745=DIRECTION('',(-1.,0.,0.));
#4746=DIRECTION('center_axis',(0.,0.,1.));
#4747=DIRECTION('ref_axis',(0.,1.,0.));
#4748=DIRECTION('',(0.,-0.707106781186548,0.707106781186547));
#4749=DIRECTION('center_axis',(0.,0.,1.));
#4750=DIRECTION('ref_axis',(0.,1.,0.));
#4751=DIRECTION('center_axis',(0.,-0.707106781186548,-0.707106781186548));
#4752=DIRECTION('ref_axis',(-1.,0.,0.));
#4753=DIRECTION('',(-1.96261557335472E-15,-0.707106781186548,0.707106781186548));
#4754=DIRECTION('',(-1.,0.,0.));
#4755=DIRECTION('',(1.,0.,0.));
#4756=DIRECTION('center_axis',(0.,0.,1.));
#4757=DIRECTION('ref_axis',(0.,-1.,0.));
#4758=DIRECTION('center_axis',(0.,0.,-1.));
#4759=DIRECTION('ref_axis',(0.,-1.,0.));
#4760=DIRECTION('center_axis',(0.,0.,1.));
#4761=DIRECTION('ref_axis',(0.,-1.,0.));
#4762=DIRECTION('center_axis',(0.,0.,1.));
#4763=DIRECTION('ref_axis',(0.,-1.,0.));
#4764=DIRECTION('',(0.,0.,1.));
#4765=DIRECTION('center_axis',(0.,0.,1.));
#4766=DIRECTION('ref_axis',(1.,0.,0.));
#4767=DIRECTION('center_axis',(0.,-1.,0.));
#4768=DIRECTION('ref_axis',(1.,0.,0.));
#4769=DIRECTION('axis',(0.,0.,1.));
#4770=DIRECTION('refdir',(1.,0.,0.));
#4771=DIRECTION('center_axis',(0.866025403784439,0.,-0.5));
#4772=DIRECTION('ref_axis',(0.5,0.,0.866025403784439));
#4773=DIRECTION('',(0.5,0.,0.866025403784439));
#4774=DIRECTION('',(0.,-1.,0.));
#4775=DIRECTION('',(0.5,0.,0.866025403784439));
#4776=DIRECTION('',(0.,-1.,0.));
#4777=DIRECTION('center_axis',(1.60246890531964E-16,0.,-1.));
#4778=DIRECTION('ref_axis',(1.,0.,1.60246890531964E-16));
#4779=DIRECTION('',(1.,0.,1.60246890531964E-16));
#4780=DIRECTION('',(0.,-1.,0.));
#4781=DIRECTION('',(1.,0.,1.60246890531964E-16));
#4782=DIRECTION('center_axis',(-0.866025403784439,0.,-0.5));
#4783=DIRECTION('ref_axis',(0.5,0.,-0.866025403784439));
#4784=DIRECTION('',(0.5,0.,-0.866025403784439));
#4785=DIRECTION('',(0.,-1.,0.));
#4786=DIRECTION('',(0.5,0.,-0.866025403784439));
#4787=DIRECTION('center_axis',(-0.866025403784439,0.,0.5));
#4788=DIRECTION('ref_axis',(-0.5,0.,-0.866025403784439));
#4789=DIRECTION('',(-0.5,0.,-0.866025403784439));
#4790=DIRECTION('',(0.,-1.,0.));
#4791=DIRECTION('',(-0.5,0.,-0.866025403784439));
#4792=DIRECTION('center_axis',(-1.60246890531964E-16,0.,1.));
#4793=DIRECTION('ref_axis',(-1.,0.,-1.60246890531964E-16));
#4794=DIRECTION('',(-1.,0.,-1.60246890531964E-16));
#4795=DIRECTION('',(0.,-1.,0.));
#4796=DIRECTION('',(-1.,0.,-1.60246890531964E-16));
#4797=DIRECTION('center_axis',(0.866025403784439,0.,0.5));
#4798=DIRECTION('ref_axis',(-0.5,0.,0.866025403784439));
#4799=DIRECTION('',(-0.5,0.,0.866025403784439));
#4800=DIRECTION('',(-0.5,0.,0.866025403784439));
#4801=DIRECTION('center_axis',(0.,-1.,0.));
#4802=DIRECTION('ref_axis',(0.,0.,-1.));
#4803=DIRECTION('center_axis',(0.,1.,0.));
#4804=DIRECTION('ref_axis',(0.,0.,1.));
#4805=DIRECTION('center_axis',(0.,-1.,0.));
#4806=DIRECTION('ref_axis',(1.,0.,0.));
#4807=DIRECTION('center_axis',(0.,-1.,0.));
#4808=DIRECTION('ref_axis',(1.,0.,0.));
#4809=DIRECTION('center_axis',(0.,-1.,0.));
#4810=DIRECTION('ref_axis',(1.,0.,0.));
#4811=DIRECTION('',(0.707106781186547,0.707106781186548,8.65956056235493E-17));
#4812=DIRECTION('center_axis',(0.,-1.,0.));
#4813=DIRECTION('ref_axis',(1.,0.,0.));
#4814=DIRECTION('center_axis',(0.,1.,0.));
#4815=DIRECTION('ref_axis',(1.,0.,0.));
#4816=DIRECTION('',(0.,1.,0.));
#4817=DIRECTION('center_axis',(0.,1.,0.));
#4818=DIRECTION('ref_axis',(1.,0.,0.));
#4819=DIRECTION('center_axis',(0.,-1.,0.));
#4820=DIRECTION('ref_axis',(1.,0.,0.));
#4821=DIRECTION('',(-0.707106781186547,0.707106781186548,-8.65956056235493E-17));
#4822=DIRECTION('center_axis',(0.,-1.,0.));
#4823=DIRECTION('ref_axis',(0.,0.,-1.));
#4824=DIRECTION('axis',(0.,0.,1.));
#4825=DIRECTION('refdir',(1.,0.,0.));
#4826=DIRECTION('center_axis',(1.,0.,0.));
#4827=DIRECTION('ref_axis',(0.,0.,-1.));
#4828=DIRECTION('',(1.,0.,0.));
#4829=DIRECTION('center_axis',(0.,1.,0.));
#4830=DIRECTION('ref_axis',(0.,0.,1.));
#4831=DIRECTION('center_axis',(0.,-1.,0.));
#4832=DIRECTION('ref_axis',(1.,0.,0.));
#4833=DIRECTION('center_axis',(0.,-1.,0.));
#4834=DIRECTION('ref_axis',(1.,0.,0.));
#4835=DIRECTION('center_axis',(0.,-1.,0.));
#4836=DIRECTION('ref_axis',(1.,0.,0.));
#4837=DIRECTION('center_axis',(0.,-1.,0.));
#4838=DIRECTION('ref_axis',(1.,0.,0.));
#4839=DIRECTION('',(0.707106781186548,0.707106781186547,8.65956056235493E-17));
#4840=DIRECTION('center_axis',(0.,-1.,0.));
#4841=DIRECTION('ref_axis',(1.,0.,0.));
#4842=DIRECTION('center_axis',(0.,-1.,0.));
#4843=DIRECTION('ref_axis',(1.,0.,0.));
#4844=DIRECTION('',(0.,1.,0.));
#4845=DIRECTION('center_axis',(0.,1.,0.));
#4846=DIRECTION('ref_axis',(1.,0.,0.));
#4847=DIRECTION('center_axis',(0.,-1.,0.));
#4848=DIRECTION('ref_axis',(1.,0.,0.));
#4849=DIRECTION('',(-0.707106781186548,0.707106781186547,-8.65956056235494E-17));
#4850=DIRECTION('center_axis',(0.,-1.,0.));
#4851=DIRECTION('ref_axis',(0.,0.,-1.));
#4852=DIRECTION('center_axis',(0.,-1.,0.));
#4853=DIRECTION('ref_axis',(1.,0.,0.));
#4854=DIRECTION('center_axis',(0.,-1.,0.));
#4855=DIRECTION('ref_axis',(1.,0.,0.));
#4856=DIRECTION('',(0.,1.,0.));
#4857=DIRECTION('axis',(0.,0.,1.));
#4858=DIRECTION('refdir',(1.,0.,0.));
#4859=DIRECTION('center_axis',(0.866025403784439,0.,-0.5));
#4860=DIRECTION('ref_axis',(0.5,0.,0.866025403784439));
#4861=DIRECTION('',(0.5,0.,0.866025403784439));
#4862=DIRECTION('',(0.,-1.,0.));
#4863=DIRECTION('',(0.5,0.,0.866025403784439));
#4864=DIRECTION('',(0.,-1.,0.));
#4865=DIRECTION('center_axis',(1.92296268638356E-16,0.,-1.));
#4866=DIRECTION('ref_axis',(1.,0.,1.92296268638356E-16));
#4867=DIRECTION('',(1.,0.,1.92296268638356E-16));
#4868=DIRECTION('',(0.,-1.,0.));
#4869=DIRECTION('',(1.,0.,1.92296268638356E-16));
#4870=DIRECTION('center_axis',(-0.866025403784439,0.,-0.5));
#4871=DIRECTION('ref_axis',(0.5,0.,-0.866025403784439));
#4872=DIRECTION('',(0.5,0.,-0.866025403784439));
#4873=DIRECTION('',(0.,-1.,0.));
#4874=DIRECTION('',(0.5,0.,-0.866025403784438));
#4875=DIRECTION('center_axis',(-0.866025403784439,0.,0.5));
#4876=DIRECTION('ref_axis',(-0.5,0.,-0.866025403784439));
#4877=DIRECTION('',(-0.5,0.,-0.866025403784439));
#4878=DIRECTION('',(0.,-1.,0.));
#4879=DIRECTION('',(-0.5,0.,-0.866025403784439));
#4880=DIRECTION('center_axis',(-1.92296268638356E-16,0.,1.));
#4881=DIRECTION('ref_axis',(-1.,0.,-1.92296268638356E-16));
#4882=DIRECTION('',(-1.,0.,-1.92296268638356E-16));
#4883=DIRECTION('',(0.,-1.,0.));
#4884=DIRECTION('',(-1.,0.,-1.92296268638356E-16));
#4885=DIRECTION('center_axis',(0.866025403784439,0.,0.5));
#4886=DIRECTION('ref_axis',(-0.5,0.,0.866025403784439));
#4887=DIRECTION('',(-0.5,0.,0.866025403784439));
#4888=DIRECTION('',(-0.5,0.,0.866025403784439));
#4889=DIRECTION('center_axis',(0.,-1.,0.));
#4890=DIRECTION('ref_axis',(0.,0.,-1.));
#4891=DIRECTION('center_axis',(0.,1.,0.));
#4892=DIRECTION('ref_axis',(0.,0.,1.));
#4893=DIRECTION('center_axis',(0.,-1.,0.));
#4894=DIRECTION('ref_axis',(1.,0.,0.));
#4895=DIRECTION('center_axis',(0.,-1.,0.));
#4896=DIRECTION('ref_axis',(1.,0.,0.));
#4897=DIRECTION('center_axis',(0.,-1.,0.));
#4898=DIRECTION('ref_axis',(1.,0.,0.));
#4899=DIRECTION('',(0.707106781186547,0.707106781186548,8.65956056235493E-17));
#4900=DIRECTION('center_axis',(0.,-1.,0.));
#4901=DIRECTION('ref_axis',(1.,0.,0.));
#4902=DIRECTION('center_axis',(0.,1.,0.));
#4903=DIRECTION('ref_axis',(1.,0.,0.));
#4904=DIRECTION('',(0.,1.,0.));
#4905=DIRECTION('center_axis',(0.,1.,0.));
#4906=DIRECTION('ref_axis',(1.,0.,0.));
#4907=DIRECTION('center_axis',(0.,-1.,0.));
#4908=DIRECTION('ref_axis',(1.,0.,0.));
#4909=DIRECTION('',(-0.707106781186547,0.707106781186548,-8.65956056235493E-17));
#4910=DIRECTION('center_axis',(0.,-1.,0.));
#4911=DIRECTION('ref_axis',(0.,0.,-1.));
#4912=DIRECTION('',(0.,0.,1.));
#4913=DIRECTION('',(1.,0.,0.));
#4914=DIRECTION('',(0.,0.,1.));
#4915=DIRECTION('',(1.,0.,0.));
#4916=DIRECTION('',(0.,0.,1.));
#4917=DIRECTION('',(2.22044604925031E-16,1.,0.));
#4918=DIRECTION('',(0.,0.,1.));
#4919=DIRECTION('',(2.22044604925031E-16,1.,0.));
#4920=DIRECTION('',(0.,0.,1.));
#4921=DIRECTION('',(1.,0.,0.));
#4922=DIRECTION('',(0.,0.,1.));
#4923=DIRECTION('',(2.22044604925031E-16,-1.,0.));
#4924=DIRECTION('',(0.,0.,1.));
#4925=DIRECTION('',(1.,0.,0.));
#4926=DIRECTION('',(0.,0.,1.));
#4927=DIRECTION('',(2.22044604925031E-16,-1.,0.));
#4928=DIRECTION('',(0.,0.,1.));
#4929=DIRECTION('',(1.,0.,0.));
#4930=DIRECTION('',(0.,0.,1.));
#4931=DIRECTION('',(1.,0.,0.));
#4932=CARTESIAN_POINT('',(0.,0.,0.));
#4933=CARTESIAN_POINT('',(0.,0.,0.));
#4934=CARTESIAN_POINT('',(0.,0.,0.));
#4935=CARTESIAN_POINT('Origin',(3.2,19.9,4.3));
#4936=CARTESIAN_POINT('',(2.86,20.,4.3));
#4937=CARTESIAN_POINT('Origin',(3.2,20.,4.3));
#4938=CARTESIAN_POINT('',(2.86,21.,4.3));
#4939=CARTESIAN_POINT('',(2.86,19.9,4.3));
#4940=CARTESIAN_POINT('Origin',(3.2,21.,4.3));
#4941=CARTESIAN_POINT('Origin',(-3.2,19.9,10.7));
#4942=CARTESIAN_POINT('',(-3.54,20.,10.7));
#4943=CARTESIAN_POINT('Origin',(-3.2,20.,10.7));
#4944=CARTESIAN_POINT('',(-3.54,21.,10.7));
#4945=CARTESIAN_POINT('',(-3.54,19.9,10.7));
#4946=CARTESIAN_POINT('Origin',(-3.2,21.,10.7));
#4947=CARTESIAN_POINT('Origin',(-3.2,19.9,4.3));
#4948=CARTESIAN_POINT('',(-3.54,20.,4.3));
#4949=CARTESIAN_POINT('Origin',(-3.2,20.,4.3));
#4950=CARTESIAN_POINT('',(-3.54,21.,4.3));
#4951=CARTESIAN_POINT('',(-3.54,19.9,4.3));
#4952=CARTESIAN_POINT('Origin',(-3.2,21.,4.3));
#4953=CARTESIAN_POINT('Origin',(3.2,19.9,10.7));
#4954=CARTESIAN_POINT('',(2.86,20.,10.7));
#4955=CARTESIAN_POINT('Origin',(3.2,20.,10.7));
#4956=CARTESIAN_POINT('',(2.86,21.,10.7));
#4957=CARTESIAN_POINT('',(2.86,19.9,10.7));
#4958=CARTESIAN_POINT('Origin',(3.2,21.,10.7));
#4959=CARTESIAN_POINT('Origin',(0.,19.9,7.5));
#4960=CARTESIAN_POINT('',(-3.01,20.,7.5));
#4961=CARTESIAN_POINT('Origin',(0.,20.,7.5));
#4962=CARTESIAN_POINT('',(-3.01,21.,7.5));
#4963=CARTESIAN_POINT('',(-3.01,19.9,7.5));
#4964=CARTESIAN_POINT('Origin',(0.,21.,7.5));
#4965=CARTESIAN_POINT('Origin',(-5.5,20.,1.));
#4966=CARTESIAN_POINT('',(-5.5,20.,13.));
#4967=CARTESIAN_POINT('',(-5.5,20.,1.));
#4968=CARTESIAN_POINT('',(-5.5,20.,13.));
#4969=CARTESIAN_POINT('',(-5.5,21.,13.));
#4970=CARTESIAN_POINT('',(-5.5,20.,13.));
#4971=CARTESIAN_POINT('',(-5.5,21.,1.));
#4972=CARTESIAN_POINT('',(-5.5,21.,13.));
#4973=CARTESIAN_POINT('',(-5.5,15.,1.));
#4974=CARTESIAN_POINT('Origin',(5.5,20.,13.));
#4975=CARTESIAN_POINT('',(5.5,20.,1.));
#4976=CARTESIAN_POINT('',(5.5,20.,13.));
#4977=CARTESIAN_POINT('',(5.5,20.,1.));
#4978=CARTESIAN_POINT('',(5.5,21.,1.));
#4979=CARTESIAN_POINT('',(5.5,15.,1.));
#4980=CARTESIAN_POINT('',(5.5,21.,13.));
#4981=CARTESIAN_POINT('',(5.5,21.,1.));
#4982=CARTESIAN_POINT('',(5.5,20.,13.));
#4983=CARTESIAN_POINT('Origin',(-5.5,20.,13.));
#4984=CARTESIAN_POINT('',(5.5,20.,13.));
#4985=CARTESIAN_POINT('',(5.5,21.,13.));
#4986=CARTESIAN_POINT('Origin',(0.,21.,7.));
#4987=CARTESIAN_POINT('',(0.,21.,1.));
#4988=CARTESIAN_POINT('Origin',(0.,20.,7.));
#4989=CARTESIAN_POINT('',(0.,20.,1.));
#4990=CARTESIAN_POINT('Origin',(3.2,-0.1,4.3));
#4991=CARTESIAN_POINT('',(2.86,0.,4.3));
#4992=CARTESIAN_POINT('Origin',(3.2,0.,4.3));
#4993=CARTESIAN_POINT('',(2.86,1.,4.3));
#4994=CARTESIAN_POINT('',(2.86,-0.1,4.3));
#4995=CARTESIAN_POINT('Origin',(3.2,1.,4.3));
#4996=CARTESIAN_POINT('Origin',(-3.2,-0.1,10.7));
#4997=CARTESIAN_POINT('',(-3.54,0.,10.7));
#4998=CARTESIAN_POINT('Origin',(-3.2,0.,10.7));
#4999=CARTESIAN_POINT('',(-3.54,1.,10.7));
#5000=CARTESIAN_POINT('',(-3.54,-0.1,10.7));
#5001=CARTESIAN_POINT('Origin',(-3.2,1.,10.7));
#5002=CARTESIAN_POINT('Origin',(-3.2,-0.1,4.3));
#5003=CARTESIAN_POINT('',(-3.54,0.,4.3));
#5004=CARTESIAN_POINT('Origin',(-3.2,0.,4.3));
#5005=CARTESIAN_POINT('',(-3.54,1.,4.3));
#5006=CARTESIAN_POINT('',(-3.54,-0.1,4.3));
#5007=CARTESIAN_POINT('Origin',(-3.2,1.,4.3));
#5008=CARTESIAN_POINT('Origin',(3.2,-0.1,10.7));
#5009=CARTESIAN_POINT('',(2.86,0.,10.7));
#5010=CARTESIAN_POINT('Origin',(3.2,0.,10.7));
#5011=CARTESIAN_POINT('',(2.86,1.,10.7));
#5012=CARTESIAN_POINT('',(2.86,-0.1,10.7));
#5013=CARTESIAN_POINT('Origin',(3.2,1.,10.7));
#5014=CARTESIAN_POINT('Origin',(0.,-0.1,7.5));
#5015=CARTESIAN_POINT('',(-3.01,0.,7.5));
#5016=CARTESIAN_POINT('Origin',(0.,0.,7.5));
#5017=CARTESIAN_POINT('',(-3.01,1.,7.5));
#5018=CARTESIAN_POINT('',(-3.01,-0.1,7.5));
#5019=CARTESIAN_POINT('Origin',(0.,1.,7.5));
#5020=CARTESIAN_POINT('Origin',(-5.5,0.,1.));
#5021=CARTESIAN_POINT('',(-5.5,0.,13.));
#5022=CARTESIAN_POINT('',(-5.5,0.,1.));
#5023=CARTESIAN_POINT('',(-5.5,0.,13.));
#5024=CARTESIAN_POINT('',(-5.5,1.,13.));
#5025=CARTESIAN_POINT('',(-5.5,0.,13.));
#5026=CARTESIAN_POINT('',(-5.5,1.,1.));
#5027=CARTESIAN_POINT('',(-5.5,1.,13.));
#5028=CARTESIAN_POINT('',(-5.5,5.,1.));
#5029=CARTESIAN_POINT('Origin',(5.5,0.,13.));
#5030=CARTESIAN_POINT('',(5.5,0.,1.));
#5031=CARTESIAN_POINT('',(5.5,0.,13.));
#5032=CARTESIAN_POINT('',(5.5,0.,1.));
#5033=CARTESIAN_POINT('',(5.5,1.,1.));
#5034=CARTESIAN_POINT('',(5.5,5.,1.));
#5035=CARTESIAN_POINT('',(5.5,1.,13.));
#5036=CARTESIAN_POINT('',(5.5,1.,1.));
#5037=CARTESIAN_POINT('',(5.5,0.,13.));
#5038=CARTESIAN_POINT('Origin',(-5.5,0.,13.));
#5039=CARTESIAN_POINT('',(5.5,0.,13.));
#5040=CARTESIAN_POINT('',(5.5,1.,13.));
#5041=CARTESIAN_POINT('Origin',(0.,1.,7.));
#5042=CARTESIAN_POINT('',(0.,1.,1.));
#5043=CARTESIAN_POINT('Origin',(0.,0.,7.));
#5044=CARTESIAN_POINT('',(0.,0.,1.));
#5045=CARTESIAN_POINT('Origin',(6.5,23.,0.));
#5046=CARTESIAN_POINT('',(6.5,23.,0.));
#5047=CARTESIAN_POINT('',(-6.5,23.,0.));
#5048=CARTESIAN_POINT('',(6.5,23.,0.));
#5049=CARTESIAN_POINT('',(-6.5,23.,1.));
#5050=CARTESIAN_POINT('',(-6.5,23.,0.));
#5051=CARTESIAN_POINT('',(6.5,23.,1.));
#5052=CARTESIAN_POINT('',(6.5,23.,1.));
#5053=CARTESIAN_POINT('',(6.5,23.,0.));
#5054=CARTESIAN_POINT('Origin',(6.5,-3.,0.));
#5055=CARTESIAN_POINT('',(6.5,-3.,0.));
#5056=CARTESIAN_POINT('',(6.5,-3.,0.));
#5057=CARTESIAN_POINT('',(6.5,-3.,1.));
#5058=CARTESIAN_POINT('',(6.5,-3.,1.));
#5059=CARTESIAN_POINT('',(6.5,-3.,0.));
#5060=CARTESIAN_POINT('Origin',(-6.5,-3.,0.));
#5061=CARTESIAN_POINT('',(-6.5,-3.,0.));
#5062=CARTESIAN_POINT('',(-6.5,-3.,0.));
#5063=CARTESIAN_POINT('',(-6.5,-3.,1.));
#5064=CARTESIAN_POINT('',(-6.5,-3.,1.));
#5065=CARTESIAN_POINT('',(-6.5,-3.,0.));
#5066=CARTESIAN_POINT('Origin',(-6.5,23.,0.));
#5067=CARTESIAN_POINT('',(-6.5,23.,0.));
#5068=CARTESIAN_POINT('',(-6.5,23.,1.));
#5069=CARTESIAN_POINT('Origin',(0.,10.,1.));
#5070=CARTESIAN_POINT('Origin',(0.,10.,0.));
#5071=CARTESIAN_POINT('',(0.,0.,0.));
#5072=CARTESIAN_POINT('Origin',(-3.2,-1.,4.3));
#5073=CARTESIAN_POINT('',(-3.625,0.,4.3));
#5074=CARTESIAN_POINT('Origin',(-3.2,0.,4.3));
#5075=CARTESIAN_POINT('',(-3.625,-1.,4.3));
#5076=CARTESIAN_POINT('',(-3.625,-1.,4.3));
#5077=CARTESIAN_POINT('Origin',(-3.2,-1.,4.3));
#5078=CARTESIAN_POINT('Origin',(-3.2,-1.,4.3));
#5079=CARTESIAN_POINT('',(-3.795,0.,4.3));
#5080=CARTESIAN_POINT('Origin',(-3.2,0.,4.3));
#5081=CARTESIAN_POINT('',(-3.795,-1.,4.3));
#5082=CARTESIAN_POINT('',(-3.795,-1.,4.3));
#5083=CARTESIAN_POINT('Origin',(-3.2,-1.,4.3));
#5084=CARTESIAN_POINT('Origin',(-3.2,0.,4.3));
#5085=CARTESIAN_POINT('Origin',(-3.2,-1.,4.3));
#5086=CARTESIAN_POINT('',(0.,0.,0.));
#5087=CARTESIAN_POINT('Origin',(-3.2,-1.,10.7));
#5088=CARTESIAN_POINT('',(-3.625,0.,10.7));
#5089=CARTESIAN_POINT('Origin',(-3.2,0.,10.7));
#5090=CARTESIAN_POINT('',(-3.625,-1.,10.7));
#5091=CARTESIAN_POINT('',(-3.625,-1.,10.7));
#5092=CARTESIAN_POINT('Origin',(-3.2,-1.,10.7));
#5093=CARTESIAN_POINT('Origin',(-3.2,-1.,10.7));
#5094=CARTESIAN_POINT('',(-3.795,0.,10.7));
#5095=CARTESIAN_POINT('Origin',(-3.2,0.,10.7));
#5096=CARTESIAN_POINT('',(-3.795,-1.,10.7));
#5097=CARTESIAN_POINT('',(-3.795,-1.,10.7));
#5098=CARTESIAN_POINT('Origin',(-3.2,-1.,10.7));
#5099=CARTESIAN_POINT('Origin',(-3.2,0.,10.7));
#5100=CARTESIAN_POINT('Origin',(-3.2,-1.,10.7));
#5101=CARTESIAN_POINT('',(0.,0.,0.));
#5102=CARTESIAN_POINT('Origin',(3.2,-1.,4.3));
#5103=CARTESIAN_POINT('',(2.775,0.,4.3));
#5104=CARTESIAN_POINT('Origin',(3.2,0.,4.3));
#5105=CARTESIAN_POINT('',(2.775,-1.,4.3));
#5106=CARTESIAN_POINT('',(2.775,-1.,4.3));
#5107=CARTESIAN_POINT('Origin',(3.2,-1.,4.3));
#5108=CARTESIAN_POINT('Origin',(3.2,-1.,4.3));
#5109=CARTESIAN_POINT('',(2.605,0.,4.3));
#5110=CARTESIAN_POINT('Origin',(3.2,0.,4.3));
#5111=CARTESIAN_POINT('',(2.605,-1.,4.3));
#5112=CARTESIAN_POINT('',(2.605,-1.,4.3));
#5113=CARTESIAN_POINT('Origin',(3.2,-1.,4.3));
#5114=CARTESIAN_POINT('Origin',(3.2,0.,4.3));
#5115=CARTESIAN_POINT('Origin',(3.2,-1.,4.3));
#5116=CARTESIAN_POINT('',(0.,0.,0.));
#5117=CARTESIAN_POINT('Origin',(3.2,-1.,10.7));
#5118=CARTESIAN_POINT('',(2.775,0.,10.7));
#5119=CARTESIAN_POINT('Origin',(3.2,0.,10.7));
#5120=CARTESIAN_POINT('',(2.775,-1.,10.7));
#5121=CARTESIAN_POINT('',(2.775,-1.,10.7));
#5122=CARTESIAN_POINT('Origin',(3.2,-1.,10.7));
#5123=CARTESIAN_POINT('Origin',(3.2,-1.,10.7));
#5124=CARTESIAN_POINT('',(2.605,0.,10.7));
#5125=CARTESIAN_POINT('Origin',(3.2,0.,10.7));
#5126=CARTESIAN_POINT('',(2.605,-1.,10.7));
#5127=CARTESIAN_POINT('',(2.605,-1.,10.7));
#5128=CARTESIAN_POINT('Origin',(3.2,-1.,10.7));
#5129=CARTESIAN_POINT('Origin',(3.2,0.,10.7));
#5130=CARTESIAN_POINT('Origin',(3.2,-1.,10.7));
#5131=CARTESIAN_POINT('',(0.,0.,0.));
#5132=CARTESIAN_POINT('Origin',(-3.2,21.,4.3));
#5133=CARTESIAN_POINT('',(-3.625,22.,4.3));
#5134=CARTESIAN_POINT('Origin',(-3.2,22.,4.3));
#5135=CARTESIAN_POINT('',(-3.625,21.,4.3));
#5136=CARTESIAN_POINT('',(-3.625,21.,4.3));
#5137=CARTESIAN_POINT('Origin',(-3.2,21.,4.3));
#5138=CARTESIAN_POINT('Origin',(-3.2,21.,4.3));
#5139=CARTESIAN_POINT('',(-3.795,22.,4.3));
#5140=CARTESIAN_POINT('Origin',(-3.2,22.,4.3));
#5141=CARTESIAN_POINT('',(-3.795,21.,4.3));
#5142=CARTESIAN_POINT('',(-3.795,21.,4.3));
#5143=CARTESIAN_POINT('Origin',(-3.2,21.,4.3));
#5144=CARTESIAN_POINT('Origin',(-3.2,22.,4.3));
#5145=CARTESIAN_POINT('Origin',(-3.2,21.,4.3));
#5146=CARTESIAN_POINT('',(0.,0.,0.));
#5147=CARTESIAN_POINT('Origin',(-3.2,21.,10.7));
#5148=CARTESIAN_POINT('',(-3.625,22.,10.7));
#5149=CARTESIAN_POINT('Origin',(-3.2,22.,10.7));
#5150=CARTESIAN_POINT('',(-3.625,21.,10.7));
#5151=CARTESIAN_POINT('',(-3.625,21.,10.7));
#5152=CARTESIAN_POINT('Origin',(-3.2,21.,10.7));
#5153=CARTESIAN_POINT('Origin',(-3.2,21.,10.7));
#5154=CARTESIAN_POINT('',(-3.795,22.,10.7));
#5155=CARTESIAN_POINT('Origin',(-3.2,22.,10.7));
#5156=CARTESIAN_POINT('',(-3.795,21.,10.7));
#5157=CARTESIAN_POINT('',(-3.795,21.,10.7));
#5158=CARTESIAN_POINT('Origin',(-3.2,21.,10.7));
#5159=CARTESIAN_POINT('Origin',(-3.2,22.,10.7));
#5160=CARTESIAN_POINT('Origin',(-3.2,21.,10.7));
#5161=CARTESIAN_POINT('',(0.,0.,0.));
#5162=CARTESIAN_POINT('Origin',(3.2,21.,4.3));
#5163=CARTESIAN_POINT('',(2.775,22.,4.3));
#5164=CARTESIAN_POINT('Origin',(3.2,22.,4.3));
#5165=CARTESIAN_POINT('',(2.775,21.,4.3));
#5166=CARTESIAN_POINT('',(2.775,21.,4.3));
#5167=CARTESIAN_POINT('Origin',(3.2,21.,4.3));
#5168=CARTESIAN_POINT('Origin',(3.2,21.,4.3));
#5169=CARTESIAN_POINT('',(2.605,22.,4.3));
#5170=CARTESIAN_POINT('Origin',(3.2,22.,4.3));
#5171=CARTESIAN_POINT('',(2.605,21.,4.3));
#5172=CARTESIAN_POINT('',(2.605,21.,4.3));
#5173=CARTESIAN_POINT('Origin',(3.2,21.,4.3));
#5174=CARTESIAN_POINT('Origin',(3.2,22.,4.3));
#5175=CARTESIAN_POINT('Origin',(3.2,21.,4.3));
#5176=CARTESIAN_POINT('',(0.,0.,0.));
#5177=CARTESIAN_POINT('Origin',(3.2,21.,10.7));
#5178=CARTESIAN_POINT('',(2.775,22.,10.7));
#5179=CARTESIAN_POINT('Origin',(3.2,22.,10.7));
#5180=CARTESIAN_POINT('',(2.775,21.,10.7));
#5181=CARTESIAN_POINT('',(2.775,21.,10.7));
#5182=CARTESIAN_POINT('Origin',(3.2,21.,10.7));
#5183=CARTESIAN_POINT('Origin',(3.2,21.,10.7));
#5184=CARTESIAN_POINT('',(2.605,22.,10.7));
#5185=CARTESIAN_POINT('Origin',(3.2,22.,10.7));
#5186=CARTESIAN_POINT('',(2.605,21.,10.7));
#5187=CARTESIAN_POINT('',(2.605,21.,10.7));
#5188=CARTESIAN_POINT('Origin',(3.2,21.,10.7));
#5189=CARTESIAN_POINT('Origin',(3.2,22.,10.7));
#5190=CARTESIAN_POINT('Origin',(3.2,21.,10.7));
#5191=CARTESIAN_POINT('',(0.,0.,0.));
#5192=CARTESIAN_POINT('',(0.,0.,0.));
#5193=CARTESIAN_POINT('Origin',(0.,0.,0.));
#5194=CARTESIAN_POINT('',(-2.05,-1.665,2.51052593825207E-16));
#5195=CARTESIAN_POINT('Origin',(0.,-1.665,0.));
#5196=CARTESIAN_POINT('',(-2.05,-1.14891252930761,-2.51052593825207E-16));
#5197=CARTESIAN_POINT('',(-2.05,0.,2.51052593825207E-16));
#5198=CARTESIAN_POINT('Origin',(0.,-1.14891252930761,0.));
#5199=CARTESIAN_POINT('Origin',(0.,0.,0.));
#5200=CARTESIAN_POINT('',(-2.05,1.14891252930761,2.51052593825207E-16));
#5201=CARTESIAN_POINT('Origin',(0.,1.14891252930761,0.));
#5202=CARTESIAN_POINT('',(-2.05,1.665,-2.51052593825207E-16));
#5203=CARTESIAN_POINT('',(-2.05,0.,2.51052593825207E-16));
#5204=CARTESIAN_POINT('Origin',(0.,1.665,0.));
#5205=CARTESIAN_POINT('Origin',(0.,0.,0.));
#5206=CARTESIAN_POINT('',(-1.43895998899814E-16,-1.76221774462768E-32,-2.35));
#5207=CARTESIAN_POINT('',(-1.43895998899814E-16,-1.76221774462768E-32,2.35));
#5208=CARTESIAN_POINT('Origin',(0.,0.,0.));
#5209=CARTESIAN_POINT('Origin',(0.,0.,0.));
#5210=CARTESIAN_POINT('',(-3.,-0.5,3.67394039744206E-16));
#5211=CARTESIAN_POINT('Origin',(0.,-0.5,0.));
#5212=CARTESIAN_POINT('',(-3.,-1.665,3.67394039744206E-16));
#5213=CARTESIAN_POINT('',(-3.,0.,3.67394039744206E-16));
#5214=CARTESIAN_POINT('Origin',(0.,-1.665,0.));
#5215=CARTESIAN_POINT('Origin',(0.,0.,0.));
#5216=CARTESIAN_POINT('',(-3.,1.665,3.67394039744206E-16));
#5217=CARTESIAN_POINT('Origin',(0.,1.665,0.));
#5218=CARTESIAN_POINT('',(-3.,0.5,-3.67394039744206E-16));
#5219=CARTESIAN_POINT('',(-3.,0.,3.67394039744206E-16));
#5220=CARTESIAN_POINT('Origin',(0.,0.5,0.));
#5221=CARTESIAN_POINT('Origin',(0.,-1.665,0.));
#5222=CARTESIAN_POINT('Origin',(0.,1.665,0.));
#5223=CARTESIAN_POINT('Origin',(3.2,0.,3.2));
#5224=CARTESIAN_POINT('',(2.6,-0.5,3.2));
#5225=CARTESIAN_POINT('Origin',(3.2,-0.5,3.2));
#5226=CARTESIAN_POINT('',(2.6,0.5,3.2));
#5227=CARTESIAN_POINT('',(2.6,0.,3.2));
#5228=CARTESIAN_POINT('Origin',(3.2,0.5,3.2));
#5229=CARTESIAN_POINT('Origin',(-3.2,0.,-3.2));
#5230=CARTESIAN_POINT('',(-3.8,-0.5,-3.2));
#5231=CARTESIAN_POINT('Origin',(-3.2,-0.5,-3.2));
#5232=CARTESIAN_POINT('',(-3.8,0.5,-3.2));
#5233=CARTESIAN_POINT('',(-3.8,0.,-3.2));
#5234=CARTESIAN_POINT('Origin',(-3.2,0.5,-3.2));
#5235=CARTESIAN_POINT('Origin',(-3.2,0.,3.2));
#5236=CARTESIAN_POINT('',(-3.8,-0.5,3.2));
#5237=CARTESIAN_POINT('Origin',(-3.2,-0.5,3.2));
#5238=CARTESIAN_POINT('',(-3.8,0.5,3.2));
#5239=CARTESIAN_POINT('',(-3.8,0.,3.2));
#5240=CARTESIAN_POINT('Origin',(-3.2,0.5,3.2));
#5241=CARTESIAN_POINT('Origin',(3.2,0.,-3.2));
#5242=CARTESIAN_POINT('',(2.6,-0.5,-3.2));
#5243=CARTESIAN_POINT('Origin',(3.2,-0.5,-3.2));
#5244=CARTESIAN_POINT('',(2.6,0.5,-3.2));
#5245=CARTESIAN_POINT('',(2.6,0.,-3.2));
#5246=CARTESIAN_POINT('Origin',(3.2,0.5,-3.2));
#5247=CARTESIAN_POINT('Origin',(-4.3,-0.5,-3.3));
#5248=CARTESIAN_POINT('',(-4.3,-0.5,-3.3));
#5249=CARTESIAN_POINT('',(-4.3,-0.5,3.3));
#5250=CARTESIAN_POINT('',(-4.3,-0.5,-3.3));
#5251=CARTESIAN_POINT('',(-4.3,0.5,3.3));
#5252=CARTESIAN_POINT('',(-4.3,-0.5,3.3));
#5253=CARTESIAN_POINT('',(-4.3,0.5,-3.3));
#5254=CARTESIAN_POINT('',(-4.3,0.5,-3.3));
#5255=CARTESIAN_POINT('',(-4.3,-0.5,-3.3));
#5256=CARTESIAN_POINT('Origin',(-3.3,-0.5,-4.3));
#5257=CARTESIAN_POINT('',(-3.3,-0.5,-4.3));
#5258=CARTESIAN_POINT('',(-3.3,-0.5,-4.3));
#5259=CARTESIAN_POINT('',(-3.3,0.5,-4.3));
#5260=CARTESIAN_POINT('',(-3.3,0.5,-4.3));
#5261=CARTESIAN_POINT('',(-3.3,-0.5,-4.3));
#5262=CARTESIAN_POINT('Origin',(3.3,-0.5,-4.3));
#5263=CARTESIAN_POINT('',(3.3,-0.5,-4.3));
#5264=CARTESIAN_POINT('',(3.3,-0.5,-4.3));
#5265=CARTESIAN_POINT('',(3.3,0.5,-4.3));
#5266=CARTESIAN_POINT('',(3.3,0.5,-4.3));
#5267=CARTESIAN_POINT('',(3.3,-0.5,-4.3));
#5268=CARTESIAN_POINT('Origin',(4.3,-0.5,-3.3));
#5269=CARTESIAN_POINT('',(4.3,-0.5,-3.3));
#5270=CARTESIAN_POINT('',(4.3,-0.5,-3.3));
#5271=CARTESIAN_POINT('',(4.3,0.5,-3.3));
#5272=CARTESIAN_POINT('',(4.3,0.5,-3.3));
#5273=CARTESIAN_POINT('',(4.3,-0.5,-3.3));
#5274=CARTESIAN_POINT('Origin',(4.3,-0.5,3.3));
#5275=CARTESIAN_POINT('',(4.3,-0.5,3.3));
#5276=CARTESIAN_POINT('',(4.3,-0.5,3.3));
#5277=CARTESIAN_POINT('',(4.3,0.5,3.3));
#5278=CARTESIAN_POINT('',(4.3,0.5,3.3));
#5279=CARTESIAN_POINT('',(4.3,-0.5,3.3));
#5280=CARTESIAN_POINT('Origin',(3.3,-0.5,4.3));
#5281=CARTESIAN_POINT('',(3.3,-0.5,4.3));
#5282=CARTESIAN_POINT('',(3.3,-0.5,4.3));
#5283=CARTESIAN_POINT('',(3.3,0.5,4.3));
#5284=CARTESIAN_POINT('',(3.3,0.5,4.3));
#5285=CARTESIAN_POINT('',(3.3,-0.5,4.3));
#5286=CARTESIAN_POINT('Origin',(-3.3,-0.5,4.3));
#5287=CARTESIAN_POINT('',(-3.3,-0.5,4.3));
#5288=CARTESIAN_POINT('',(-3.3,-0.5,4.3));
#5289=CARTESIAN_POINT('',(-3.3,0.5,4.3));
#5290=CARTESIAN_POINT('',(-3.3,0.5,4.3));
#5291=CARTESIAN_POINT('',(-3.3,-0.5,4.3));
#5292=CARTESIAN_POINT('Origin',(-4.3,-0.5,3.3));
#5293=CARTESIAN_POINT('',(-4.3,-0.5,3.3));
#5294=CARTESIAN_POINT('',(-4.3,0.5,3.3));
#5295=CARTESIAN_POINT('Origin',(0.,0.5,0.));
#5296=CARTESIAN_POINT('Origin',(0.,-0.5,0.));
#5297=CARTESIAN_POINT('',(0.,0.,0.));
#5298=CARTESIAN_POINT('Origin',(0.,0.,0.));
#5299=CARTESIAN_POINT('',(-1.8,-0.85,-2.20436423846524E-16));
#5300=CARTESIAN_POINT('Origin',(0.,-0.85,0.));
#5301=CARTESIAN_POINT('',(-1.8,0.85,-2.20436423846524E-16));
#5302=CARTESIAN_POINT('',(-1.8,0.,-2.20436423846524E-16));
#5303=CARTESIAN_POINT('Origin',(0.,0.85,0.));
#5304=CARTESIAN_POINT('Origin',(2.19089023002066,0.85,0.));
#5305=CARTESIAN_POINT('',(2.19089023002066,0.85,0.));
#5306=CARTESIAN_POINT('Origin',(0.,0.85,0.));
#5307=CARTESIAN_POINT('Origin',(3.99680288865056E-15,0.,0.));
#5308=CARTESIAN_POINT('',(3.85290688975075E-15,-1.76221774462768E-32,2.35));
#5309=CARTESIAN_POINT('',(3.85290688975075E-15,-1.76221774462768E-32,-2.35));
#5310=CARTESIAN_POINT('Origin',(3.99680288865056E-15,0.,0.));
#5311=CARTESIAN_POINT('',(2.19089023002066,-0.85,0.));
#5312=CARTESIAN_POINT('Origin',(0.,-0.85,0.));
#5313=CARTESIAN_POINT('Origin',(1.8,-0.85,0.));
#5314=CARTESIAN_POINT('Origin',(0.,1.55,0.));
#5315=CARTESIAN_POINT('',(1.42894191624432,1.8,0.825000000000001));
#5316=CARTESIAN_POINT('',(1.53744468918255,1.55,0.598968970568896));
#5317=CARTESIAN_POINT('Ctrl Pts',(1.42894191624432,1.8,0.825000000000001));
#5318=CARTESIAN_POINT('Ctrl Pts',(1.44466308895875,1.8,0.797770130104052));
#5319=CARTESIAN_POINT('Ctrl Pts',(1.46055812562105,1.79370633789704,0.768258557763732));
#5320=CARTESIAN_POINT('Ctrl Pts',(1.48824888379079,1.76817777258318,0.713138492740816));
#5321=CARTESIAN_POINT('Ctrl Pts',(1.50008999307766,1.74894552961493,0.687551581002689));
#5322=CARTESIAN_POINT('Ctrl Pts',(1.51812136280714,1.70460745840382,0.646764802471699));
#5323=CARTESIAN_POINT('Ctrl Pts',(1.52552758004446,1.67652816181843,0.628833667319578));
#5324=CARTESIAN_POINT('Ctrl Pts',(1.53516661651472,1.61494799959182,0.604921184808251));
#5325=CARTESIAN_POINT('Ctrl Pts',(1.53744468918255,1.58144291640553,0.598968970568896));
#5326=CARTESIAN_POINT('Ctrl Pts',(1.53744468918255,1.55,0.598968970568896));
#5327=CARTESIAN_POINT('',(1.42894191624432,1.3,0.825000000000001));
#5328=CARTESIAN_POINT('Ctrl Pts',(1.42894191624432,1.3,0.825000000000001));
#5329=CARTESIAN_POINT('Ctrl Pts',(1.4132207435299,1.3,0.852229869895949));
#5330=CARTESIAN_POINT('Ctrl Pts',(1.39561049050871,1.30629366210296,0.880751161609749));
#5331=CARTESIAN_POINT('Ctrl Pts',(1.36172049302549,1.33182222741682,0.932292094146256));
#5332=CARTESIAN_POINT('Ctrl Pts',(1.34548213209931,1.35105447038507,0.955340251466734));
#5333=CARTESIAN_POINT('Ctrl Pts',(1.31917543061769,1.39539254159618,0.99134926498299));
#5334=CARTESIAN_POINT('Ctrl Pts',(1.30734972067592,1.42347183818157,1.00672880483252));
#5335=CARTESIAN_POINT('Ctrl Pts',(1.29146042158868,1.48505200040818,1.02703269653942));
#5336=CARTESIAN_POINT('Ctrl Pts',(1.28744468918255,1.51855708359447,1.03198167246111));
#5337=CARTESIAN_POINT('Ctrl Pts',(1.28744468918255,1.58144291640553,1.03198167246111));
#5338=CARTESIAN_POINT('Ctrl Pts',(1.29146042158868,1.61494799959182,1.02703269653942));
#5339=CARTESIAN_POINT('Ctrl Pts',(1.30734972067592,1.67652816181843,1.00672880483252));
#5340=CARTESIAN_POINT('Ctrl Pts',(1.31917543061769,1.70460745840382,0.991349264982991));
#5341=CARTESIAN_POINT('Ctrl Pts',(1.34548213209931,1.74894552961493,0.955340251466735));
#5342=CARTESIAN_POINT('Ctrl Pts',(1.36172049302549,1.76817777258318,0.932292094146256));
#5343=CARTESIAN_POINT('Ctrl Pts',(1.39561049050871,1.79370633789704,0.880751161609749));
#5344=CARTESIAN_POINT('Ctrl Pts',(1.4132207435299,1.8,0.85222986989595));
#5345=CARTESIAN_POINT('Ctrl Pts',(1.42894191624432,1.8,0.825000000000001));
#5346=CARTESIAN_POINT('Ctrl Pts',(1.53744468918255,1.55,0.598968970568896));
#5347=CARTESIAN_POINT('Ctrl Pts',(1.53744468918255,1.51855708359447,0.598968970568896));
#5348=CARTESIAN_POINT('Ctrl Pts',(1.53516661651472,1.48505200040818,0.60492118480825));
#5349=CARTESIAN_POINT('Ctrl Pts',(1.52552758004446,1.42347183818157,0.628833667319578));
#5350=CARTESIAN_POINT('Ctrl Pts',(1.51812136280714,1.39539254159618,0.646764802471699));
#5351=CARTESIAN_POINT('Ctrl Pts',(1.50008999307766,1.35105447038507,0.687551581002689));
#5352=CARTESIAN_POINT('Ctrl Pts',(1.48824888379079,1.33182222741682,0.713138492740816));
#5353=CARTESIAN_POINT('Ctrl Pts',(1.46055812562105,1.30629366210296,0.768258557763732));
#5354=CARTESIAN_POINT('Ctrl Pts',(1.44466308895875,1.3,0.797770130104052));
#5355=CARTESIAN_POINT('Ctrl Pts',(1.42894191624432,1.3,0.825000000000001));
#5356=CARTESIAN_POINT('',(0.59736109069228,1.55,0.0562114519197835));
#5357=CARTESIAN_POINT('',(0.125,1.55,-0.21650635094611));
#5358=CARTESIAN_POINT('Ctrl Pts',(0.59736109069228,1.55,0.0562114519197835));
#5359=CARTESIAN_POINT('Ctrl Pts',(0.59736109069228,1.58183602855499,0.0562114519197835));
#5360=CARTESIAN_POINT('Ctrl Pts',(0.596809586309859,1.61548166177648,0.0633319361811907));
#5361=CARTESIAN_POINT('Ctrl Pts',(0.593243052195919,1.67693412158597,0.0908585874761106));
#5362=CARTESIAN_POINT('Ctrl Pts',(0.590063593315144,1.70478184753241,0.111151766652641));
#5363=CARTESIAN_POINT('Ctrl Pts',(0.579820497891285,1.74874496453875,0.15600214762839));
#5364=CARTESIAN_POINT('Ctrl Pts',(0.572042315803119,1.76792916820474,0.183678633836535));
#5365=CARTESIAN_POINT('Ctrl Pts',(0.549947124580676,1.79356669468566,0.241926459727039));
#5366=CARTESIAN_POINT('Ctrl Pts',(0.53551402125728,1.8,0.27246250701687));
#5367=CARTESIAN_POINT('Ctrl Pts',(0.503716463284046,1.8,0.32753749298313));
#5368=CARTESIAN_POINT('Ctrl Pts',(0.484488022261586,1.79356669468566,0.355304950761552));
#5369=CARTESIAN_POINT('Ctrl Pts',(0.445091520936419,1.76792916820474,0.403563860606914));
#5370=CARTESIAN_POINT('Ctrl Pts',(0.425012071836758,1.74874496453875,0.4241382069946));
#5371=CARTESIAN_POINT('Ctrl Pts',(0.391292050254278,1.70478184753241,0.455434178332924));
#5372=CARTESIAN_POINT('Ctrl Pts',(0.375307371004241,1.67693412158597,0.468334260082228));
#5373=CARTESIAN_POINT('Ctrl Pts',(0.353251858758695,1.61548166177647,0.485186294875824));
#5374=CARTESIAN_POINT('Ctrl Pts',(0.347361090692279,1.58183602855499,0.489224153812003));
#5375=CARTESIAN_POINT('Ctrl Pts',(0.347361090692279,1.51816397144501,0.489224153812003));
#5376=CARTESIAN_POINT('Ctrl Pts',(0.353251858758695,1.48451833822352,0.485186294875824));
#5377=CARTESIAN_POINT('Ctrl Pts',(0.375307371004241,1.42306587841403,0.468334260082228));
#5378=CARTESIAN_POINT('Ctrl Pts',(0.391292050254278,1.39521815246759,0.455434178332924));
#5379=CARTESIAN_POINT('Ctrl Pts',(0.425012071836758,1.35125503546125,0.4241382069946));
#5380=CARTESIAN_POINT('Ctrl Pts',(0.445091520936418,1.33207083179526,0.403563860606914));
#5381=CARTESIAN_POINT('Ctrl Pts',(0.484488022261586,1.30643330531434,0.355304950761552));
#5382=CARTESIAN_POINT('Ctrl Pts',(0.503716463284046,1.3,0.32753749298313));
#5383=CARTESIAN_POINT('Ctrl Pts',(0.53551402125728,1.3,0.27246250701687));
#5384=CARTESIAN_POINT('Ctrl Pts',(0.549947124580676,1.30643330531434,0.241926459727039));
#5385=CARTESIAN_POINT('Ctrl Pts',(0.572042315803119,1.33207083179526,0.183678633836535));
#5386=CARTESIAN_POINT('Ctrl Pts',(0.579820497891285,1.35125503546125,0.15600214762839));
#5387=CARTESIAN_POINT('Ctrl Pts',(0.590063593315144,1.39521815246759,0.111151766652641));
#5388=CARTESIAN_POINT('Ctrl Pts',(0.593243052195919,1.42306587841403,0.0908585874761105));
#5389=CARTESIAN_POINT('Ctrl Pts',(0.596809586309859,1.48451833822352,0.0633319361811906));
#5390=CARTESIAN_POINT('Ctrl Pts',(0.59736109069228,1.51816397144501,0.0562114519197835));
#5391=CARTESIAN_POINT('Ctrl Pts',(0.59736109069228,1.55,0.0562114519197835));
#5392=CARTESIAN_POINT('Origin',(0.,1.55,0.));
#5393=CARTESIAN_POINT('',(-0.347361090692279,1.55,-0.489224153812003));
#5394=CARTESIAN_POINT('Ctrl Pts',(-0.347361090692279,1.55,-0.489224153812003));
#5395=CARTESIAN_POINT('Ctrl Pts',(-0.347361090692279,1.51816397144501,-0.489224153812003));
#5396=CARTESIAN_POINT('Ctrl Pts',(-0.353251858758695,1.48451833822352,-0.485186294875824));
#5397=CARTESIAN_POINT('Ctrl Pts',(-0.375307371004241,1.42306587841403,-0.468334260082228));
#5398=CARTESIAN_POINT('Ctrl Pts',(-0.391292050254278,1.39521815246759,-0.455434178332924));
#5399=CARTESIAN_POINT('Ctrl Pts',(-0.425012071836758,1.35125503546125,-0.4241382069946));
#5400=CARTESIAN_POINT('Ctrl Pts',(-0.445091520936419,1.33207083179526,-0.403563860606914));
#5401=CARTESIAN_POINT('Ctrl Pts',(-0.484488022261586,1.30643330531434,-0.355304950761552));
#5402=CARTESIAN_POINT('Ctrl Pts',(-0.503716463284046,1.3,-0.32753749298313));
#5403=CARTESIAN_POINT('Ctrl Pts',(-0.53551402125728,1.3,-0.27246250701687));
#5404=CARTESIAN_POINT('Ctrl Pts',(-0.549947124580676,1.30643330531434,-0.241926459727039));
#5405=CARTESIAN_POINT('Ctrl Pts',(-0.572042315803119,1.33207083179526,-0.183678633836535));
#5406=CARTESIAN_POINT('Ctrl Pts',(-0.579820497891285,1.35125503546125,-0.15600214762839));
#5407=CARTESIAN_POINT('Ctrl Pts',(-0.590063593315144,1.39521815246759,-0.111151766652641));
#5408=CARTESIAN_POINT('Ctrl Pts',(-0.593243052195918,1.42306587841403,-0.0908585874761106));
#5409=CARTESIAN_POINT('Ctrl Pts',(-0.596809586309859,1.48451833822352,-0.0633319361811906));
#5410=CARTESIAN_POINT('Ctrl Pts',(-0.597361090692279,1.51816397144501,-0.0562114519197835));
#5411=CARTESIAN_POINT('Ctrl Pts',(-0.597361090692279,1.58183602855499,-0.0562114519197835));
#5412=CARTESIAN_POINT('Ctrl Pts',(-0.596809586309859,1.61548166177647,-0.0633319361811905));
#5413=CARTESIAN_POINT('Ctrl Pts',(-0.593243052195918,1.67693412158597,-0.0908585874761104));
#5414=CARTESIAN_POINT('Ctrl Pts',(-0.590063593315144,1.70478184753241,-0.111151766652641));
#5415=CARTESIAN_POINT('Ctrl Pts',(-0.579820497891285,1.74874496453875,-0.15600214762839));
#5416=CARTESIAN_POINT('Ctrl Pts',(-0.572042315803118,1.76792916820474,-0.183678633836535));
#5417=CARTESIAN_POINT('Ctrl Pts',(-0.549947124580676,1.79356669468566,-0.241926459727039));
#5418=CARTESIAN_POINT('Ctrl Pts',(-0.53551402125728,1.8,-0.27246250701687));
#5419=CARTESIAN_POINT('Ctrl Pts',(-0.503716463284046,1.8,-0.32753749298313));
#5420=CARTESIAN_POINT('Ctrl Pts',(-0.484488022261586,1.79356669468566,-0.355304950761552));
#5421=CARTESIAN_POINT('Ctrl Pts',(-0.445091520936419,1.76792916820474,-0.403563860606914));
#5422=CARTESIAN_POINT('Ctrl Pts',(-0.425012071836758,1.74874496453875,-0.4241382069946));
#5423=CARTESIAN_POINT('Ctrl Pts',(-0.391292050254278,1.70478184753241,-0.455434178332924));
#5424=CARTESIAN_POINT('Ctrl Pts',(-0.375307371004241,1.67693412158597,-0.468334260082228));
#5425=CARTESIAN_POINT('Ctrl Pts',(-0.353251858758695,1.61548166177648,-0.485186294875824));
#5426=CARTESIAN_POINT('Ctrl Pts',(-0.347361090692279,1.58183602855499,-0.489224153812003));
#5427=CARTESIAN_POINT('Ctrl Pts',(-0.347361090692279,1.55,-0.489224153812003));
#5428=CARTESIAN_POINT('',(-1.28744468918255,1.55,-1.03198167246111));
#5429=CARTESIAN_POINT('',(0.125,1.55,-0.21650635094611));
#5430=CARTESIAN_POINT('',(-1.42894191624432,1.3,-0.825000000000001));
#5431=CARTESIAN_POINT('Ctrl Pts',(-1.42894191624432,1.3,-0.825000000000001));
#5432=CARTESIAN_POINT('Ctrl Pts',(-1.4132207435299,1.3,-0.852229869895949));
#5433=CARTESIAN_POINT('Ctrl Pts',(-1.39561049050871,1.30629366210296,-0.880751161609749));
#5434=CARTESIAN_POINT('Ctrl Pts',(-1.36172049302549,1.33182222741682,-0.932292094146256));
#5435=CARTESIAN_POINT('Ctrl Pts',(-1.34548213209931,1.35105447038507,-0.955340251466735));
#5436=CARTESIAN_POINT('Ctrl Pts',(-1.31917543061769,1.39539254159618,-0.991349264982991));
#5437=CARTESIAN_POINT('Ctrl Pts',(-1.30734972067592,1.42347183818157,-1.00672880483252));
#5438=CARTESIAN_POINT('Ctrl Pts',(-1.29146042158868,1.48505200040818,-1.02703269653942));
#5439=CARTESIAN_POINT('Ctrl Pts',(-1.28744468918255,1.51855708359447,-1.03198167246111));
#5440=CARTESIAN_POINT('Ctrl Pts',(-1.28744468918255,1.55,-1.03198167246111));
#5441=CARTESIAN_POINT('',(-1.42894191624432,1.8,-0.825000000000001));
#5442=CARTESIAN_POINT('Ctrl Pts',(-1.42894191624432,1.8,-0.825000000000001));
#5443=CARTESIAN_POINT('Ctrl Pts',(-1.44466308895875,1.8,-0.797770130104052));
#5444=CARTESIAN_POINT('Ctrl Pts',(-1.46055812562105,1.79370633789704,-0.768258557763732));
#5445=CARTESIAN_POINT('Ctrl Pts',(-1.48824888379079,1.76817777258318,-0.713138492740816));
#5446=CARTESIAN_POINT('Ctrl Pts',(-1.50008999307766,1.74894552961493,-0.687551581002689));
#5447=CARTESIAN_POINT('Ctrl Pts',(-1.51812136280714,1.70460745840382,-0.646764802471699));
#5448=CARTESIAN_POINT('Ctrl Pts',(-1.52552758004446,1.67652816181843,-0.628833667319578));
#5449=CARTESIAN_POINT('Ctrl Pts',(-1.53516661651472,1.61494799959182,-0.60492118480825));
#5450=CARTESIAN_POINT('Ctrl Pts',(-1.53744468918255,1.58144291640553,-0.598968970568896));
#5451=CARTESIAN_POINT('Ctrl Pts',(-1.53744468918255,1.51855708359447,-0.598968970568896));
#5452=CARTESIAN_POINT('Ctrl Pts',(-1.53516661651472,1.48505200040818,-0.60492118480825));
#5453=CARTESIAN_POINT('Ctrl Pts',(-1.52552758004446,1.42347183818157,-0.628833667319578));
#5454=CARTESIAN_POINT('Ctrl Pts',(-1.51812136280714,1.39539254159618,-0.646764802471699));
#5455=CARTESIAN_POINT('Ctrl Pts',(-1.50008999307766,1.35105447038507,-0.687551581002689));
#5456=CARTESIAN_POINT('Ctrl Pts',(-1.48824888379079,1.33182222741682,-0.713138492740816));
#5457=CARTESIAN_POINT('Ctrl Pts',(-1.46055812562105,1.30629366210296,-0.768258557763732));
#5458=CARTESIAN_POINT('Ctrl Pts',(-1.44466308895875,1.3,-0.797770130104052));
#5459=CARTESIAN_POINT('Ctrl Pts',(-1.42894191624432,1.3,-0.825000000000001));
#5460=CARTESIAN_POINT('Ctrl Pts',(-1.28744468918255,1.55,-1.03198167246111));
#5461=CARTESIAN_POINT('Ctrl Pts',(-1.28744468918255,1.58144291640553,-1.03198167246111));
#5462=CARTESIAN_POINT('Ctrl Pts',(-1.29146042158868,1.61494799959182,-1.02703269653942));
#5463=CARTESIAN_POINT('Ctrl Pts',(-1.30734972067592,1.67652816181843,-1.00672880483252));
#5464=CARTESIAN_POINT('Ctrl Pts',(-1.31917543061769,1.70460745840382,-0.991349264982991));
#5465=CARTESIAN_POINT('Ctrl Pts',(-1.34548213209931,1.74894552961493,-0.955340251466734));
#5466=CARTESIAN_POINT('Ctrl Pts',(-1.36172049302549,1.76817777258318,-0.932292094146256));
#5467=CARTESIAN_POINT('Ctrl Pts',(-1.39561049050871,1.79370633789704,-0.880751161609749));
#5468=CARTESIAN_POINT('Ctrl Pts',(-1.4132207435299,1.8,-0.852229869895949));
#5469=CARTESIAN_POINT('Ctrl Pts',(-1.42894191624432,1.8,-0.825000000000001));
#5470=CARTESIAN_POINT('Origin',(0.,1.55,0.));
#5471=CARTESIAN_POINT('',(-1.65,0.85,-2.02066721859313E-16));
#5472=CARTESIAN_POINT('Origin',(0.,0.85,0.));
#5473=CARTESIAN_POINT('',(-1.65,2.25,-2.02066721859313E-16));
#5474=CARTESIAN_POINT('',(-1.65,1.55,-2.02066721859313E-16));
#5475=CARTESIAN_POINT('Origin',(0.,2.25,0.));
#5476=CARTESIAN_POINT('',(-1.42894191624432,1.3,0.825));
#5477=CARTESIAN_POINT('',(-1.42894191624432,1.8,0.825));
#5478=CARTESIAN_POINT('Ctrl Pts',(-1.42894191624432,1.3,0.825));
#5479=CARTESIAN_POINT('Ctrl Pts',(-1.44466308895875,1.3,0.797770130104051));
#5480=CARTESIAN_POINT('Ctrl Pts',(-1.46055812562105,1.30629366210296,0.768258557763731));
#5481=CARTESIAN_POINT('Ctrl Pts',(-1.48824888379079,1.33182222741682,0.713138492740815));
#5482=CARTESIAN_POINT('Ctrl Pts',(-1.50008999307766,1.35105447038507,0.687551581002688));
#5483=CARTESIAN_POINT('Ctrl Pts',(-1.51812136280714,1.39539254159618,0.646764802471698));
#5484=CARTESIAN_POINT('Ctrl Pts',(-1.52552758004446,1.42347183818157,0.628833667319577));
#5485=CARTESIAN_POINT('Ctrl Pts',(-1.53516661651472,1.48505200040818,0.604921184808249));
#5486=CARTESIAN_POINT('Ctrl Pts',(-1.53744468918255,1.51855708359447,0.598968970568895));
#5487=CARTESIAN_POINT('Ctrl Pts',(-1.53744468918255,1.58144291640553,0.598968970568895));
#5488=CARTESIAN_POINT('Ctrl Pts',(-1.53516661651472,1.61494799959182,0.604921184808249));
#5489=CARTESIAN_POINT('Ctrl Pts',(-1.52552758004446,1.67652816181843,0.628833667319577));
#5490=CARTESIAN_POINT('Ctrl Pts',(-1.51812136280714,1.70460745840382,0.646764802471698));
#5491=CARTESIAN_POINT('Ctrl Pts',(-1.50008999307766,1.74894552961493,0.687551581002688));
#5492=CARTESIAN_POINT('Ctrl Pts',(-1.48824888379079,1.76817777258318,0.713138492740815));
#5493=CARTESIAN_POINT('Ctrl Pts',(-1.46055812562105,1.79370633789704,0.768258557763731));
#5494=CARTESIAN_POINT('Ctrl Pts',(-1.44466308895875,1.8,0.797770130104051));
#5495=CARTESIAN_POINT('Ctrl Pts',(-1.42894191624432,1.8,0.825));
#5496=CARTESIAN_POINT('',(-1.28744468918255,1.55,1.03198167246111));
#5497=CARTESIAN_POINT('Ctrl Pts',(-1.42894191624432,1.8,0.825));
#5498=CARTESIAN_POINT('Ctrl Pts',(-1.4132207435299,1.8,0.852229869895948));
#5499=CARTESIAN_POINT('Ctrl Pts',(-1.39561049050871,1.79370633789704,0.880751161609747));
#5500=CARTESIAN_POINT('Ctrl Pts',(-1.36172049302549,1.76817777258318,0.932292094146255));
#5501=CARTESIAN_POINT('Ctrl Pts',(-1.34548213209931,1.74894552961493,0.955340251466733));
#5502=CARTESIAN_POINT('Ctrl Pts',(-1.31917543061769,1.70460745840382,0.991349264982989));
#5503=CARTESIAN_POINT('Ctrl Pts',(-1.30734972067592,1.67652816181843,1.00672880483252));
#5504=CARTESIAN_POINT('Ctrl Pts',(-1.29146042158868,1.61494799959182,1.02703269653942));
#5505=CARTESIAN_POINT('Ctrl Pts',(-1.28744468918255,1.58144291640553,1.03198167246111));
#5506=CARTESIAN_POINT('Ctrl Pts',(-1.28744468918255,1.55,1.03198167246111));
#5507=CARTESIAN_POINT('Ctrl Pts',(-1.28744468918255,1.55,1.03198167246111));
#5508=CARTESIAN_POINT('Ctrl Pts',(-1.28744468918255,1.51855708359447,1.03198167246111));
#5509=CARTESIAN_POINT('Ctrl Pts',(-1.29146042158868,1.48505200040818,1.02703269653942));
#5510=CARTESIAN_POINT('Ctrl Pts',(-1.30734972067592,1.42347183818157,1.00672880483252));
#5511=CARTESIAN_POINT('Ctrl Pts',(-1.31917543061769,1.39539254159618,0.99134926498299));
#5512=CARTESIAN_POINT('Ctrl Pts',(-1.34548213209931,1.35105447038508,0.955340251466733));
#5513=CARTESIAN_POINT('Ctrl Pts',(-1.36172049302549,1.33182222741682,0.932292094146255));
#5514=CARTESIAN_POINT('Ctrl Pts',(-1.39561049050871,1.30629366210296,0.880751161609748));
#5515=CARTESIAN_POINT('Ctrl Pts',(-1.4132207435299,1.3,0.852229869895949));
#5516=CARTESIAN_POINT('Ctrl Pts',(-1.42894191624432,1.3,0.825));
#5517=CARTESIAN_POINT('',(1.42894191624432,1.8,-0.825));
#5518=CARTESIAN_POINT('',(1.42894191624432,1.3,-0.825));
#5519=CARTESIAN_POINT('Ctrl Pts',(1.42894191624432,1.8,-0.825));
#5520=CARTESIAN_POINT('Ctrl Pts',(1.4132207435299,1.8,-0.852229869895949));
#5521=CARTESIAN_POINT('Ctrl Pts',(1.39561049050871,1.79370633789704,-0.880751161609748));
#5522=CARTESIAN_POINT('Ctrl Pts',(1.36172049302549,1.76817777258318,-0.932292094146255));
#5523=CARTESIAN_POINT('Ctrl Pts',(1.34548213209931,1.74894552961493,-0.955340251466734));
#5524=CARTESIAN_POINT('Ctrl Pts',(1.31917543061769,1.70460745840382,-0.99134926498299));
#5525=CARTESIAN_POINT('Ctrl Pts',(1.30734972067592,1.67652816181843,-1.00672880483252));
#5526=CARTESIAN_POINT('Ctrl Pts',(1.29146042158868,1.61494799959182,-1.02703269653942));
#5527=CARTESIAN_POINT('Ctrl Pts',(1.28744468918255,1.58144291640553,-1.03198167246111));
#5528=CARTESIAN_POINT('Ctrl Pts',(1.28744468918255,1.51855708359447,-1.03198167246111));
#5529=CARTESIAN_POINT('Ctrl Pts',(1.29146042158868,1.48505200040818,-1.02703269653942));
#5530=CARTESIAN_POINT('Ctrl Pts',(1.30734972067592,1.42347183818157,-1.00672880483252));
#5531=CARTESIAN_POINT('Ctrl Pts',(1.31917543061769,1.39539254159618,-0.99134926498299));
#5532=CARTESIAN_POINT('Ctrl Pts',(1.34548213209931,1.35105447038507,-0.955340251466734));
#5533=CARTESIAN_POINT('Ctrl Pts',(1.36172049302549,1.33182222741682,-0.932292094146255));
#5534=CARTESIAN_POINT('Ctrl Pts',(1.39561049050871,1.30629366210296,-0.880751161609748));
#5535=CARTESIAN_POINT('Ctrl Pts',(1.4132207435299,1.3,-0.852229869895948));
#5536=CARTESIAN_POINT('Ctrl Pts',(1.42894191624432,1.3,-0.825));
#5537=CARTESIAN_POINT('',(1.53744468918255,1.55,-0.598968970568895));
#5538=CARTESIAN_POINT('Ctrl Pts',(1.42894191624432,1.3,-0.825));
#5539=CARTESIAN_POINT('Ctrl Pts',(1.44466308895875,1.3,-0.797770130104051));
#5540=CARTESIAN_POINT('Ctrl Pts',(1.46055812562105,1.30629366210296,-0.768258557763731));
#5541=CARTESIAN_POINT('Ctrl Pts',(1.48824888379079,1.33182222741682,-0.713138492740815));
#5542=CARTESIAN_POINT('Ctrl Pts',(1.50008999307766,1.35105447038507,-0.687551581002688));
#5543=CARTESIAN_POINT('Ctrl Pts',(1.51812136280714,1.39539254159618,-0.646764802471698));
#5544=CARTESIAN_POINT('Ctrl Pts',(1.52552758004446,1.42347183818157,-0.628833667319577));
#5545=CARTESIAN_POINT('Ctrl Pts',(1.53516661651472,1.48505200040818,-0.604921184808249));
#5546=CARTESIAN_POINT('Ctrl Pts',(1.53744468918255,1.51855708359447,-0.598968970568895));
#5547=CARTESIAN_POINT('Ctrl Pts',(1.53744468918255,1.55,-0.598968970568895));
#5548=CARTESIAN_POINT('Ctrl Pts',(1.53744468918255,1.55,-0.598968970568895));
#5549=CARTESIAN_POINT('Ctrl Pts',(1.53744468918255,1.58144291640553,-0.598968970568895));
#5550=CARTESIAN_POINT('Ctrl Pts',(1.53516661651472,1.61494799959182,-0.604921184808249));
#5551=CARTESIAN_POINT('Ctrl Pts',(1.52552758004446,1.67652816181843,-0.628833667319577));
#5552=CARTESIAN_POINT('Ctrl Pts',(1.51812136280714,1.70460745840382,-0.646764802471698));
#5553=CARTESIAN_POINT('Ctrl Pts',(1.50008999307766,1.74894552961493,-0.687551581002688));
#5554=CARTESIAN_POINT('Ctrl Pts',(1.48824888379079,1.76817777258318,-0.713138492740815));
#5555=CARTESIAN_POINT('Ctrl Pts',(1.46055812562105,1.79370633789704,-0.768258557763731));
#5556=CARTESIAN_POINT('Ctrl Pts',(1.44466308895875,1.8,-0.797770130104051));
#5557=CARTESIAN_POINT('Ctrl Pts',(1.42894191624432,1.8,-0.825));
#5558=CARTESIAN_POINT('',(0.,1.3,-1.65));
#5559=CARTESIAN_POINT('',(0.,1.8,-1.65));
#5560=CARTESIAN_POINT('Ctrl Pts',(1.38777878078145E-17,1.3,-1.65));
#5561=CARTESIAN_POINT('Ctrl Pts',(0.0314423454288489,1.3,-1.65));
#5562=CARTESIAN_POINT('Ctrl Pts',(0.0649476351123396,1.30629366210296,-1.64900971937348));
#5563=CARTESIAN_POINT('Ctrl Pts',(0.126528390765307,1.33182222741682,-1.64543058688707));
#5564=CARTESIAN_POINT('Ctrl Pts',(0.154607860978348,1.35105447038507,-1.64289183246942));
#5565=CARTESIAN_POINT('Ctrl Pts',(0.198945932189457,1.39539254159618,-1.63811406745469));
#5566=CARTESIAN_POINT('Ctrl Pts',(0.218177859368546,1.42347183818157,-1.63556247215209));
#5567=CARTESIAN_POINT('Ctrl Pts',(0.243706194926033,1.48505200040818,-1.63195388134767));
#5568=CARTESIAN_POINT('Ctrl Pts',(0.25,1.51855708359447,-1.63095064303001));
#5569=CARTESIAN_POINT('Ctrl Pts',(0.25,1.58144291640553,-1.63095064303001));
#5570=CARTESIAN_POINT('Ctrl Pts',(0.243706194926033,1.61494799959182,-1.63195388134767));
#5571=CARTESIAN_POINT('Ctrl Pts',(0.218177859368546,1.67652816181843,-1.63556247215209));
#5572=CARTESIAN_POINT('Ctrl Pts',(0.198945932189457,1.70460745840382,-1.63811406745469));
#5573=CARTESIAN_POINT('Ctrl Pts',(0.154607860978349,1.74894552961493,-1.64289183246942));
#5574=CARTESIAN_POINT('Ctrl Pts',(0.126528390765307,1.76817777258318,-1.64543058688707));
#5575=CARTESIAN_POINT('Ctrl Pts',(0.0649476351123398,1.79370633789704,-1.64900971937348));
#5576=CARTESIAN_POINT('Ctrl Pts',(0.031442345428849,1.8,-1.65));
#5577=CARTESIAN_POINT('Ctrl Pts',(7.63278329429795E-17,1.8,-1.65));
#5578=CARTESIAN_POINT('',(-0.25,1.55,-1.63095064303001));
#5579=CARTESIAN_POINT('Ctrl Pts',(9.0205620750794E-17,1.8,-1.65));
#5580=CARTESIAN_POINT('Ctrl Pts',(-0.0314423454288488,1.8,-1.65));
#5581=CARTESIAN_POINT('Ctrl Pts',(-0.0649476351123396,1.79370633789704,
-1.64900971937348));
#5582=CARTESIAN_POINT('Ctrl Pts',(-0.126528390765307,1.76817777258318,-1.64543058688707));
#5583=CARTESIAN_POINT('Ctrl Pts',(-0.154607860978348,1.74894552961493,-1.64289183246942));
#5584=CARTESIAN_POINT('Ctrl Pts',(-0.198945932189456,1.70460745840382,-1.63811406745469));
#5585=CARTESIAN_POINT('Ctrl Pts',(-0.218177859368546,1.67652816181843,-1.63556247215209));
#5586=CARTESIAN_POINT('Ctrl Pts',(-0.243706194926033,1.61494799959182,-1.63195388134767));
#5587=CARTESIAN_POINT('Ctrl Pts',(-0.25,1.58144291640553,-1.63095064303001));
#5588=CARTESIAN_POINT('Ctrl Pts',(-0.25,1.55,-1.63095064303001));
#5589=CARTESIAN_POINT('Ctrl Pts',(-0.25,1.55,-1.63095064303001));
#5590=CARTESIAN_POINT('Ctrl Pts',(-0.25,1.51855708359447,-1.63095064303001));
#5591=CARTESIAN_POINT('Ctrl Pts',(-0.243706194926033,1.48505200040818,-1.63195388134767));
#5592=CARTESIAN_POINT('Ctrl Pts',(-0.218177859368546,1.42347183818157,-1.63556247215209));
#5593=CARTESIAN_POINT('Ctrl Pts',(-0.198945932189457,1.39539254159618,-1.63811406745469));
#5594=CARTESIAN_POINT('Ctrl Pts',(-0.154607860978349,1.35105447038507,-1.64289183246942));
#5595=CARTESIAN_POINT('Ctrl Pts',(-0.126528390765307,1.33182222741682,-1.64543058688707));
#5596=CARTESIAN_POINT('Ctrl Pts',(-0.0649476351123398,1.30629366210296,
-1.64900971937348));
#5597=CARTESIAN_POINT('Ctrl Pts',(-0.031442345428849,1.3,-1.65));
#5598=CARTESIAN_POINT('Ctrl Pts',(-4.85722573273506E-17,1.3,-1.65));
#5599=CARTESIAN_POINT('',(0.,1.8,1.65));
#5600=CARTESIAN_POINT('',(0.,1.3,1.65));
#5601=CARTESIAN_POINT('Ctrl Pts',(8.32667268468867E-17,1.8,1.65));
#5602=CARTESIAN_POINT('Ctrl Pts',(0.031442345428849,1.8,1.65));
#5603=CARTESIAN_POINT('Ctrl Pts',(0.0649476351123398,1.79370633789704,1.64900971937348));
#5604=CARTESIAN_POINT('Ctrl Pts',(0.126528390765307,1.76817777258318,1.64543058688707));
#5605=CARTESIAN_POINT('Ctrl Pts',(0.154607860978349,1.74894552961493,1.64289183246942));
#5606=CARTESIAN_POINT('Ctrl Pts',(0.198945932189457,1.70460745840382,1.63811406745469));
#5607=CARTESIAN_POINT('Ctrl Pts',(0.218177859368546,1.67652816181843,1.63556247215209));
#5608=CARTESIAN_POINT('Ctrl Pts',(0.243706194926033,1.61494799959182,1.63195388134767));
#5609=CARTESIAN_POINT('Ctrl Pts',(0.25,1.58144291640553,1.63095064303001));
#5610=CARTESIAN_POINT('Ctrl Pts',(0.25,1.51855708359447,1.63095064303001));
#5611=CARTESIAN_POINT('Ctrl Pts',(0.243706194926033,1.48505200040818,1.63195388134767));
#5612=CARTESIAN_POINT('Ctrl Pts',(0.218177859368546,1.42347183818157,1.63556247215209));
#5613=CARTESIAN_POINT('Ctrl Pts',(0.198945932189457,1.39539254159618,1.63811406745469));
#5614=CARTESIAN_POINT('Ctrl Pts',(0.154607860978348,1.35105447038507,1.64289183246942));
#5615=CARTESIAN_POINT('Ctrl Pts',(0.126528390765307,1.33182222741682,1.64543058688707));
#5616=CARTESIAN_POINT('Ctrl Pts',(0.0649476351123397,1.30629366210296,1.64900971937348));
#5617=CARTESIAN_POINT('Ctrl Pts',(0.0314423454288488,1.3,1.65));
#5618=CARTESIAN_POINT('Ctrl Pts',(-1.38777878078145E-17,1.3,1.65));
#5619=CARTESIAN_POINT('',(-0.25,1.55,1.63095064303001));
#5620=CARTESIAN_POINT('Ctrl Pts',(-5.55111512312578E-17,1.3,1.65));
#5621=CARTESIAN_POINT('Ctrl Pts',(-0.031442345428849,1.3,1.65));
#5622=CARTESIAN_POINT('Ctrl Pts',(-0.0649476351123398,1.30629366210296,
1.64900971937348));
#5623=CARTESIAN_POINT('Ctrl Pts',(-0.126528390765307,1.33182222741682,1.64543058688707));
#5624=CARTESIAN_POINT('Ctrl Pts',(-0.154607860978349,1.35105447038507,1.64289183246942));
#5625=CARTESIAN_POINT('Ctrl Pts',(-0.198945932189457,1.39539254159618,1.63811406745469));
#5626=CARTESIAN_POINT('Ctrl Pts',(-0.218177859368546,1.42347183818157,1.63556247215209));
#5627=CARTESIAN_POINT('Ctrl Pts',(-0.243706194926033,1.48505200040818,1.63195388134767));
#5628=CARTESIAN_POINT('Ctrl Pts',(-0.25,1.51855708359447,1.63095064303001));
#5629=CARTESIAN_POINT('Ctrl Pts',(-0.25,1.55,1.63095064303001));
#5630=CARTESIAN_POINT('Ctrl Pts',(-0.25,1.55,1.63095064303001));
#5631=CARTESIAN_POINT('Ctrl Pts',(-0.25,1.58144291640553,1.63095064303001));
#5632=CARTESIAN_POINT('Ctrl Pts',(-0.243706194926033,1.61494799959182,1.63195388134767));
#5633=CARTESIAN_POINT('Ctrl Pts',(-0.218177859368546,1.67652816181843,1.63556247215209));
#5634=CARTESIAN_POINT('Ctrl Pts',(-0.198945932189456,1.70460745840382,1.63811406745469));
#5635=CARTESIAN_POINT('Ctrl Pts',(-0.154607860978348,1.74894552961493,1.64289183246942));
#5636=CARTESIAN_POINT('Ctrl Pts',(-0.126528390765307,1.76817777258318,1.64543058688707));
#5637=CARTESIAN_POINT('Ctrl Pts',(-0.0649476351123396,1.79370633789704,
1.64900971937348));
#5638=CARTESIAN_POINT('Ctrl Pts',(-0.0314423454288488,1.8,1.65));
#5639=CARTESIAN_POINT('Ctrl Pts',(7.63278329429795E-17,1.8,1.65));
#5640=CARTESIAN_POINT('Origin',(0.,1.55,0.));
#5641=CARTESIAN_POINT('',(-0.34736109069228,1.55,0.489224153812002));
#5642=CARTESIAN_POINT('',(0.125,1.55,0.21650635094611));
#5643=CARTESIAN_POINT('Ctrl Pts',(-0.34736109069228,1.55,0.489224153812002));
#5644=CARTESIAN_POINT('Ctrl Pts',(-0.34736109069228,1.58183602855499,0.489224153812002));
#5645=CARTESIAN_POINT('Ctrl Pts',(-0.353251858758695,1.61548166177648,0.485186294875824));
#5646=CARTESIAN_POINT('Ctrl Pts',(-0.375307371004242,1.67693412158597,0.468334260082228));
#5647=CARTESIAN_POINT('Ctrl Pts',(-0.391292050254279,1.70478184753241,0.455434178332924));
#5648=CARTESIAN_POINT('Ctrl Pts',(-0.425012071836758,1.74874496453875,0.424138206994599));
#5649=CARTESIAN_POINT('Ctrl Pts',(-0.445091520936419,1.76792916820474,0.403563860606914));
#5650=CARTESIAN_POINT('Ctrl Pts',(-0.484488022261587,1.79356669468566,0.355304950761552));
#5651=CARTESIAN_POINT('Ctrl Pts',(-0.503716463284046,1.8,0.32753749298313));
#5652=CARTESIAN_POINT('Ctrl Pts',(-0.535514021257281,1.8,0.27246250701687));
#5653=CARTESIAN_POINT('Ctrl Pts',(-0.549947124580677,1.79356669468566,0.241926459727038));
#5654=CARTESIAN_POINT('Ctrl Pts',(-0.572042315803119,1.76792916820474,0.183678633836535));
#5655=CARTESIAN_POINT('Ctrl Pts',(-0.579820497891285,1.74874496453875,0.156002147628389));
#5656=CARTESIAN_POINT('Ctrl Pts',(-0.590063593315144,1.70478184753241,0.11115176665264));
#5657=CARTESIAN_POINT('Ctrl Pts',(-0.593243052195919,1.67693412158597,0.0908585874761102));
#5658=CARTESIAN_POINT('Ctrl Pts',(-0.596809586309859,1.61548166177648,0.0633319361811903));
#5659=CARTESIAN_POINT('Ctrl Pts',(-0.59736109069228,1.58183602855499,0.0562114519197831));
#5660=CARTESIAN_POINT('Ctrl Pts',(-0.59736109069228,1.51816397144501,0.0562114519197831));
#5661=CARTESIAN_POINT('Ctrl Pts',(-0.596809586309859,1.48451833822352,0.0633319361811902));
#5662=CARTESIAN_POINT('Ctrl Pts',(-0.593243052195919,1.42306587841403,0.0908585874761101));
#5663=CARTESIAN_POINT('Ctrl Pts',(-0.590063593315144,1.39521815246759,0.11115176665264));
#5664=CARTESIAN_POINT('Ctrl Pts',(-0.579820497891285,1.35125503546125,0.156002147628389));
#5665=CARTESIAN_POINT('Ctrl Pts',(-0.572042315803119,1.33207083179526,0.183678633836535));
#5666=CARTESIAN_POINT('Ctrl Pts',(-0.549947124580676,1.30643330531434,0.241926459727038));
#5667=CARTESIAN_POINT('Ctrl Pts',(-0.535514021257281,1.3,0.27246250701687));
#5668=CARTESIAN_POINT('Ctrl Pts',(-0.503716463284046,1.3,0.32753749298313));
#5669=CARTESIAN_POINT('Ctrl Pts',(-0.484488022261587,1.30643330531434,0.355304950761552));
#5670=CARTESIAN_POINT('Ctrl Pts',(-0.445091520936419,1.33207083179526,0.403563860606914));
#5671=CARTESIAN_POINT('Ctrl Pts',(-0.425012071836758,1.35125503546125,0.424138206994599));
#5672=CARTESIAN_POINT('Ctrl Pts',(-0.391292050254279,1.39521815246759,0.455434178332924));
#5673=CARTESIAN_POINT('Ctrl Pts',(-0.375307371004241,1.42306587841403,0.468334260082228));
#5674=CARTESIAN_POINT('Ctrl Pts',(-0.353251858758695,1.48451833822352,0.485186294875824));
#5675=CARTESIAN_POINT('Ctrl Pts',(-0.34736109069228,1.51816397144501,0.489224153812002));
#5676=CARTESIAN_POINT('Ctrl Pts',(-0.34736109069228,1.55,0.489224153812002));
#5677=CARTESIAN_POINT('Origin',(0.,1.55,0.));
#5678=CARTESIAN_POINT('',(0.59736109069228,1.55,-0.0562114519197831));
#5679=CARTESIAN_POINT('Ctrl Pts',(0.59736109069228,1.55,-0.0562114519197831));
#5680=CARTESIAN_POINT('Ctrl Pts',(0.59736109069228,1.51816397144501,-0.0562114519197831));
#5681=CARTESIAN_POINT('Ctrl Pts',(0.596809586309859,1.48451833822352,-0.0633319361811902));
#5682=CARTESIAN_POINT('Ctrl Pts',(0.593243052195919,1.42306587841403,-0.0908585874761101));
#5683=CARTESIAN_POINT('Ctrl Pts',(0.590063593315144,1.39521815246759,-0.11115176665264));
#5684=CARTESIAN_POINT('Ctrl Pts',(0.579820497891285,1.35125503546125,-0.156002147628389));
#5685=CARTESIAN_POINT('Ctrl Pts',(0.572042315803119,1.33207083179526,-0.183678633836535));
#5686=CARTESIAN_POINT('Ctrl Pts',(0.549947124580677,1.30643330531434,-0.241926459727038));
#5687=CARTESIAN_POINT('Ctrl Pts',(0.535514021257281,1.3,-0.27246250701687));
#5688=CARTESIAN_POINT('Ctrl Pts',(0.503716463284046,1.3,-0.32753749298313));
#5689=CARTESIAN_POINT('Ctrl Pts',(0.484488022261587,1.30643330531434,-0.355304950761552));
#5690=CARTESIAN_POINT('Ctrl Pts',(0.445091520936419,1.33207083179526,-0.403563860606914));
#5691=CARTESIAN_POINT('Ctrl Pts',(0.425012071836758,1.35125503546125,-0.424138206994599));
#5692=CARTESIAN_POINT('Ctrl Pts',(0.391292050254279,1.39521815246759,-0.455434178332924));
#5693=CARTESIAN_POINT('Ctrl Pts',(0.375307371004241,1.42306587841403,-0.468334260082228));
#5694=CARTESIAN_POINT('Ctrl Pts',(0.353251858758695,1.48451833822352,-0.485186294875824));
#5695=CARTESIAN_POINT('Ctrl Pts',(0.34736109069228,1.51816397144501,-0.489224153812002));
#5696=CARTESIAN_POINT('Ctrl Pts',(0.34736109069228,1.58183602855499,-0.489224153812002));
#5697=CARTESIAN_POINT('Ctrl Pts',(0.353251858758695,1.61548166177647,-0.485186294875824));
#5698=CARTESIAN_POINT('Ctrl Pts',(0.375307371004241,1.67693412158597,-0.468334260082228));
#5699=CARTESIAN_POINT('Ctrl Pts',(0.391292050254279,1.70478184753241,-0.455434178332924));
#5700=CARTESIAN_POINT('Ctrl Pts',(0.425012071836758,1.74874496453875,-0.424138206994599));
#5701=CARTESIAN_POINT('Ctrl Pts',(0.445091520936419,1.76792916820474,-0.403563860606914));
#5702=CARTESIAN_POINT('Ctrl Pts',(0.484488022261587,1.79356669468566,-0.355304950761552));
#5703=CARTESIAN_POINT('Ctrl Pts',(0.503716463284046,1.8,-0.32753749298313));
#5704=CARTESIAN_POINT('Ctrl Pts',(0.535514021257281,1.8,-0.27246250701687));
#5705=CARTESIAN_POINT('Ctrl Pts',(0.549947124580677,1.79356669468566,-0.241926459727038));
#5706=CARTESIAN_POINT('Ctrl Pts',(0.572042315803119,1.76792916820474,-0.183678633836535));
#5707=CARTESIAN_POINT('Ctrl Pts',(0.579820497891285,1.74874496453875,-0.156002147628389));
#5708=CARTESIAN_POINT('Ctrl Pts',(0.590063593315144,1.70478184753241,-0.111151766652641));
#5709=CARTESIAN_POINT('Ctrl Pts',(0.593243052195919,1.67693412158597,-0.0908585874761104));
#5710=CARTESIAN_POINT('Ctrl Pts',(0.596809586309859,1.61548166177648,-0.0633319361811903));
#5711=CARTESIAN_POINT('Ctrl Pts',(0.59736109069228,1.58183602855499,-0.0562114519197831));
#5712=CARTESIAN_POINT('Ctrl Pts',(0.59736109069228,1.55,-0.0562114519197831));
#5713=CARTESIAN_POINT('',(0.125,1.55,0.21650635094611));
#5714=CARTESIAN_POINT('Origin',(0.,1.55,0.));
#5715=CARTESIAN_POINT('',(-0.25,1.55,-0.545435605731786));
#5716=CARTESIAN_POINT('',(-0.25,1.55,0.));
#5717=CARTESIAN_POINT('Ctrl Pts',(-0.25,1.55,-0.545435605731786));
#5718=CARTESIAN_POINT('Ctrl Pts',(-0.25,1.58183602855499,-0.545435605731786));
#5719=CARTESIAN_POINT('Ctrl Pts',(-0.243557727551164,1.61548166177648,-0.548518231057014));
#5720=CARTESIAN_POINT('Ctrl Pts',(-0.217935681191677,1.67693412158597,-0.559192847558338));
#5721=CARTESIAN_POINT('Ctrl Pts',(-0.198771543060865,1.70478184753241,-0.566585944985565));
#5722=CARTESIAN_POINT('Ctrl Pts',(-0.154808426054527,1.74874496453875,-0.580140354622989));
#5723=CARTESIAN_POINT('Ctrl Pts',(-0.1269507948667,1.76792916820474,-0.587242494443449));
#5724=CARTESIAN_POINT('Ctrl Pts',(-0.0654591023190899,1.79356669468566,
-0.597231410488591));
#5725=CARTESIAN_POINT('Ctrl Pts',(-0.0317975579732349,1.8,-0.6));
#5726=CARTESIAN_POINT('Ctrl Pts',(0.0317975579732349,1.8,-0.6));
#5727=CARTESIAN_POINT('Ctrl Pts',(0.0654591023190898,1.79356669468566,-0.597231410488591));
#5728=CARTESIAN_POINT('Ctrl Pts',(0.1269507948667,1.76792916820474,-0.587242494443449));
#5729=CARTESIAN_POINT('Ctrl Pts',(0.154808426054527,1.74874496453875,-0.580140354622989));
#5730=CARTESIAN_POINT('Ctrl Pts',(0.198771543060865,1.70478184753241,-0.566585944985565));
#5731=CARTESIAN_POINT('Ctrl Pts',(0.217935681191677,1.67693412158597,-0.559192847558338));
#5732=CARTESIAN_POINT('Ctrl Pts',(0.243557727551164,1.61548166177648,-0.548518231057014));
#5733=CARTESIAN_POINT('Ctrl Pts',(0.25,1.58183602855499,-0.545435605731786));
#5734=CARTESIAN_POINT('Ctrl Pts',(0.25,1.51816397144501,-0.545435605731786));
#5735=CARTESIAN_POINT('Ctrl Pts',(0.243557727551164,1.48451833822352,-0.548518231057014));
#5736=CARTESIAN_POINT('Ctrl Pts',(0.217935681191677,1.42306587841403,-0.559192847558338));
#5737=CARTESIAN_POINT('Ctrl Pts',(0.198771543060865,1.39521815246759,-0.566585944985565));
#5738=CARTESIAN_POINT('Ctrl Pts',(0.154808426054527,1.35125503546125,-0.580140354622989));
#5739=CARTESIAN_POINT('Ctrl Pts',(0.1269507948667,1.33207083179526,-0.587242494443449));
#5740=CARTESIAN_POINT('Ctrl Pts',(0.0654591023190899,1.30643330531434,-0.597231410488591));
#5741=CARTESIAN_POINT('Ctrl Pts',(0.0317975579732349,1.3,-0.6));
#5742=CARTESIAN_POINT('Ctrl Pts',(-0.0317975579732349,1.3,-0.6));
#5743=CARTESIAN_POINT('Ctrl Pts',(-0.0654591023190899,1.30643330531434,
-0.597231410488591));
#5744=CARTESIAN_POINT('Ctrl Pts',(-0.1269507948667,1.33207083179526,-0.587242494443449));
#5745=CARTESIAN_POINT('Ctrl Pts',(-0.154808426054527,1.35125503546125,-0.580140354622989));
#5746=CARTESIAN_POINT('Ctrl Pts',(-0.198771543060865,1.39521815246759,-0.566585944985565));
#5747=CARTESIAN_POINT('Ctrl Pts',(-0.217935681191677,1.42306587841403,-0.559192847558338));
#5748=CARTESIAN_POINT('Ctrl Pts',(-0.243557727551164,1.48451833822352,-0.548518231057014));
#5749=CARTESIAN_POINT('Ctrl Pts',(-0.25,1.51816397144501,-0.545435605731786));
#5750=CARTESIAN_POINT('Ctrl Pts',(-0.25,1.55,-0.545435605731786));
#5751=CARTESIAN_POINT('Origin',(0.,1.55,0.));
#5752=CARTESIAN_POINT('',(-0.25,1.55,0.545435605731786));
#5753=CARTESIAN_POINT('Ctrl Pts',(-0.25,1.55,0.545435605731786));
#5754=CARTESIAN_POINT('Ctrl Pts',(-0.25,1.51816397144501,0.545435605731786));
#5755=CARTESIAN_POINT('Ctrl Pts',(-0.243557727551164,1.48451833822352,0.548518231057014));
#5756=CARTESIAN_POINT('Ctrl Pts',(-0.217935681191677,1.42306587841403,0.559192847558338));
#5757=CARTESIAN_POINT('Ctrl Pts',(-0.198771543060865,1.39521815246759,0.566585944985565));
#5758=CARTESIAN_POINT('Ctrl Pts',(-0.154808426054527,1.35125503546125,0.580140354622989));
#5759=CARTESIAN_POINT('Ctrl Pts',(-0.1269507948667,1.33207083179526,0.587242494443449));
#5760=CARTESIAN_POINT('Ctrl Pts',(-0.0654591023190899,1.30643330531434,
0.597231410488591));
#5761=CARTESIAN_POINT('Ctrl Pts',(-0.0317975579732349,1.3,0.6));
#5762=CARTESIAN_POINT('Ctrl Pts',(0.0317975579732349,1.3,0.6));
#5763=CARTESIAN_POINT('Ctrl Pts',(0.0654591023190899,1.30643330531434,0.597231410488591));
#5764=CARTESIAN_POINT('Ctrl Pts',(0.1269507948667,1.33207083179526,0.587242494443449));
#5765=CARTESIAN_POINT('Ctrl Pts',(0.154808426054527,1.35125503546125,0.580140354622989));
#5766=CARTESIAN_POINT('Ctrl Pts',(0.198771543060865,1.39521815246759,0.566585944985565));
#5767=CARTESIAN_POINT('Ctrl Pts',(0.217935681191677,1.42306587841403,0.559192847558338));
#5768=CARTESIAN_POINT('Ctrl Pts',(0.243557727551164,1.48451833822352,0.548518231057014));
#5769=CARTESIAN_POINT('Ctrl Pts',(0.25,1.51816397144501,0.545435605731786));
#5770=CARTESIAN_POINT('Ctrl Pts',(0.25,1.58183602855499,0.545435605731786));
#5771=CARTESIAN_POINT('Ctrl Pts',(0.243557727551164,1.61548166177648,0.548518231057014));
#5772=CARTESIAN_POINT('Ctrl Pts',(0.217935681191677,1.67693412158597,0.559192847558338));
#5773=CARTESIAN_POINT('Ctrl Pts',(0.198771543060865,1.70478184753241,0.566585944985565));
#5774=CARTESIAN_POINT('Ctrl Pts',(0.154808426054527,1.74874496453875,0.580140354622989));
#5775=CARTESIAN_POINT('Ctrl Pts',(0.1269507948667,1.76792916820474,0.587242494443449));
#5776=CARTESIAN_POINT('Ctrl Pts',(0.0654591023190898,1.79356669468566,0.597231410488591));
#5777=CARTESIAN_POINT('Ctrl Pts',(0.0317975579732349,1.8,0.6));
#5778=CARTESIAN_POINT('Ctrl Pts',(-0.0317975579732349,1.8,0.6));
#5779=CARTESIAN_POINT('Ctrl Pts',(-0.0654591023190898,1.79356669468566,
0.597231410488591));
#5780=CARTESIAN_POINT('Ctrl Pts',(-0.1269507948667,1.76792916820474,0.587242494443449));
#5781=CARTESIAN_POINT('Ctrl Pts',(-0.154808426054527,1.74874496453875,0.580140354622989));
#5782=CARTESIAN_POINT('Ctrl Pts',(-0.198771543060865,1.70478184753241,0.566585944985565));
#5783=CARTESIAN_POINT('Ctrl Pts',(-0.217935681191677,1.67693412158597,0.559192847558339));
#5784=CARTESIAN_POINT('Ctrl Pts',(-0.243557727551164,1.61548166177648,0.548518231057014));
#5785=CARTESIAN_POINT('Ctrl Pts',(-0.25,1.58183602855499,0.545435605731786));
#5786=CARTESIAN_POINT('Ctrl Pts',(-0.25,1.55,0.545435605731786));
#5787=CARTESIAN_POINT('',(-0.25,1.55,0.));
#5788=CARTESIAN_POINT('Origin',(1.65,2.25,0.));
#5789=CARTESIAN_POINT('',(-0.6,2.25,-7.34788079488412E-17));
#5790=CARTESIAN_POINT('Origin',(0.,2.25,0.));
#5791=CARTESIAN_POINT('Origin',(1.75,0.85,0.));
#5792=CARTESIAN_POINT('',(-1.75,0.85,-2.14313189850787E-16));
#5793=CARTESIAN_POINT('Origin',(0.,0.85,0.));
#5794=CARTESIAN_POINT('Origin',(0.,0.,0.));
#5795=CARTESIAN_POINT('',(-1.75,-0.85,-2.14313189850787E-16));
#5796=CARTESIAN_POINT('Origin',(0.,-0.85,0.));
#5797=CARTESIAN_POINT('',(-1.75,0.,-2.14313189850787E-16));
#5798=CARTESIAN_POINT('Origin',(0.6,-0.85,0.));
#5799=CARTESIAN_POINT('',(-0.6,-0.85,-7.34788079488412E-17));
#5800=CARTESIAN_POINT('Origin',(0.,-0.85,0.));
#5801=CARTESIAN_POINT('Origin',(0.,0.7,0.));
#5802=CARTESIAN_POINT('',(-0.6,0.7,-7.34788079488412E-17));
#5803=CARTESIAN_POINT('',(0.,0.,0.));
#5804=CARTESIAN_POINT('',(0.,0.,0.));
#5805=CARTESIAN_POINT('',(0.,0.,0.));
#5806=CARTESIAN_POINT('Origin',(0.,0.,0.));
#5807=CARTESIAN_POINT('',(-0.42,0.16,5.14351655641888E-17));
#5808=CARTESIAN_POINT('Origin',(0.,0.16,0.));
#5809=CARTESIAN_POINT('',(-0.42,0.,5.14351655641888E-17));
#5810=CARTESIAN_POINT('',(-0.42,0.,5.14351655641888E-17));
#5811=CARTESIAN_POINT('Origin',(0.,0.,0.));
#5812=CARTESIAN_POINT('Origin',(0.,0.,0.));
#5813=CARTESIAN_POINT('',(-0.8,0.16,9.79717439317883E-17));
#5814=CARTESIAN_POINT('Origin',(0.,0.16,0.));
#5815=CARTESIAN_POINT('',(-0.8,0.,9.79717439317883E-17));
#5816=CARTESIAN_POINT('',(-0.8,0.,9.79717439317883E-17));
#5817=CARTESIAN_POINT('Origin',(0.,0.,0.));
#5818=CARTESIAN_POINT('Origin',(0.,0.16,0.));
#5819=CARTESIAN_POINT('Origin',(0.,0.,0.));
#5820=CARTESIAN_POINT('',(0.,0.,0.));
#5821=CARTESIAN_POINT('Origin',(0.6,0.8,0.));
#5822=CARTESIAN_POINT('',(-0.6,0.8,-7.34788079488412E-17));
#5823=CARTESIAN_POINT('Origin',(0.,0.8,0.));
#5824=CARTESIAN_POINT('Origin',(0.,0.775,0.));
#5825=CARTESIAN_POINT('',(-0.65,0.75,-7.9602041944578E-17));
#5826=CARTESIAN_POINT('Origin',(0.,0.75,0.));
#5827=CARTESIAN_POINT('',(-0.625,0.775,-7.65404249467096E-17));
#5828=CARTESIAN_POINT('Origin',(0.,0.39,0.));
#5829=CARTESIAN_POINT('',(-0.65,0.0299999999999998,-7.9602041944578E-17));
#5830=CARTESIAN_POINT('Origin',(0.,0.0299999999999998,0.));
#5831=CARTESIAN_POINT('',(-0.65,0.39,-7.9602041944578E-17));
#5832=CARTESIAN_POINT('Origin',(0.,0.0150000000000001,0.));
#5833=CARTESIAN_POINT('',(-0.62,5.89805981832114E-17,-7.59281015471359E-17));
#5834=CARTESIAN_POINT('Origin',(0.,0.,0.));
#5835=CARTESIAN_POINT('',(-0.635,0.0150000000000001,-7.77650717458569E-17));
#5836=CARTESIAN_POINT('Origin',(0.42,0.,0.));
#5837=CARTESIAN_POINT('',(-0.42,-3.46944695195361E-18,-5.14351655641888E-17));
#5838=CARTESIAN_POINT('Origin',(0.,0.,0.));
#5839=CARTESIAN_POINT('Origin',(0.,-0.02,0.));
#5840=CARTESIAN_POINT('',(-0.3933,-0.0534000000000001,4.81653586104654E-17));
#5841=CARTESIAN_POINT('Origin',(0.,-0.0534000000000001,0.));
#5842=CARTESIAN_POINT('',(-0.41,-0.02,-5.02105187650415E-17));
#5843=CARTESIAN_POINT('Origin',(0.,-1.48,0.));
#5844=CARTESIAN_POINT('',(-0.3933,-2.9267,4.81653586104654E-17));
#5845=CARTESIAN_POINT('Origin',(0.,-2.9267,0.));
#5846=CARTESIAN_POINT('',(-0.3933,-1.48,-4.81653586104654E-17));
#5847=CARTESIAN_POINT('Origin',(0.,-2.96,0.));
#5848=CARTESIAN_POINT('',(-0.32,-3.,-3.91886975727153E-17));
#5849=CARTESIAN_POINT('Origin',(0.,-3.,0.));
#5850=CARTESIAN_POINT('',(-0.36,-2.96,-4.40872847693047E-17));
#5851=CARTESIAN_POINT('Origin',(0.,-3.,0.));
#5852=CARTESIAN_POINT('Origin',(0.173205080756888,-0.8,-0.3));
#5853=CARTESIAN_POINT('',(0.346410161513775,-0.8,0.));
#5854=CARTESIAN_POINT('',(0.173205080756888,-0.8,-0.3));
#5855=CARTESIAN_POINT('',(0.346410161513775,-0.8,0.));
#5856=CARTESIAN_POINT('',(0.173205080756888,-1.28,-0.3));
#5857=CARTESIAN_POINT('',(0.173205080756888,-0.8,-0.3));
#5858=CARTESIAN_POINT('',(0.346410161513775,-1.28,0.));
#5859=CARTESIAN_POINT('',(0.346410161513775,-1.28,0.));
#5860=CARTESIAN_POINT('',(0.346410161513775,-0.8,0.));
#5861=CARTESIAN_POINT('Origin',(-0.173205080756888,-0.8,-0.3));
#5862=CARTESIAN_POINT('',(-0.173205080756888,-0.8,-0.3));
#5863=CARTESIAN_POINT('',(0.173205080756888,-0.8,-0.3));
#5864=CARTESIAN_POINT('',(-0.173205080756888,-1.28,-0.3));
#5865=CARTESIAN_POINT('',(-0.173205080756888,-0.8,-0.3));
#5866=CARTESIAN_POINT('',(0.173205080756888,-1.28,-0.3));
#5867=CARTESIAN_POINT('Origin',(-0.346410161513775,-0.8,-5.55111512312578E-17));
#5868=CARTESIAN_POINT('',(-0.346410161513775,-0.8,-4.24230095489963E-17));
#5869=CARTESIAN_POINT('',(-0.173205080756888,-0.8,-0.3));
#5870=CARTESIAN_POINT('',(-0.346410161513775,-1.28,-5.55111512312578E-17));
#5871=CARTESIAN_POINT('',(-0.346410161513775,-0.8,-4.24230095489963E-17));
#5872=CARTESIAN_POINT('',(-0.173205080756888,-1.28,-0.3));
#5873=CARTESIAN_POINT('Origin',(-0.173205080756888,-0.8,0.3));
#5874=CARTESIAN_POINT('',(-0.173205080756888,-0.8,0.3));
#5875=CARTESIAN_POINT('',(-0.346410161513775,-0.8,-4.24230095489963E-17));
#5876=CARTESIAN_POINT('',(-0.173205080756888,-1.28,0.3));
#5877=CARTESIAN_POINT('',(-0.173205080756888,-0.8,0.3));
#5878=CARTESIAN_POINT('',(-0.346410161513775,-1.28,-4.24230095489963E-17));
#5879=CARTESIAN_POINT('Origin',(0.173205080756888,-0.8,0.3));
#5880=CARTESIAN_POINT('',(0.173205080756888,-0.8,0.3));
#5881=CARTESIAN_POINT('',(-0.173205080756888,-0.8,0.3));
#5882=CARTESIAN_POINT('',(0.173205080756888,-1.28,0.3));
#5883=CARTESIAN_POINT('',(0.173205080756888,-0.8,0.3));
#5884=CARTESIAN_POINT('',(-0.173205080756888,-1.28,0.3));
#5885=CARTESIAN_POINT('Origin',(0.346410161513775,-0.8,0.));
#5886=CARTESIAN_POINT('',(0.173205080756888,-0.8,0.3));
#5887=CARTESIAN_POINT('',(0.173205080756888,-1.28,0.3));
#5888=CARTESIAN_POINT('Origin',(0.,-0.8,-5.55111512312578E-17));
#5889=CARTESIAN_POINT('Origin',(0.,-1.28,-5.55111512312578E-17));
#5890=CARTESIAN_POINT('',(0.,0.,0.));
#5891=CARTESIAN_POINT('',(0.,0.,0.));
#5892=CARTESIAN_POINT('',(0.,0.,0.));
#5893=CARTESIAN_POINT('',(0.,0.,0.));
#5894=CARTESIAN_POINT('',(0.,0.,0.));
#5895=CARTESIAN_POINT('',(0.,0.,0.));
#5896=CARTESIAN_POINT('',(0.,0.,0.));
#5897=CARTESIAN_POINT('',(0.,0.,0.));
#5898=CARTESIAN_POINT('',(0.,0.,0.));
#5899=CARTESIAN_POINT('',(0.,-0.5,7.5));
#5900=CARTESIAN_POINT('',(-3.2,-1.,4.3));
#5901=CARTESIAN_POINT('',(-3.2,-1.16,4.3));
#5902=CARTESIAN_POINT('',(-3.2,-1.,10.7));
#5903=CARTESIAN_POINT('',(-3.2,-1.16,10.7));
#5904=CARTESIAN_POINT('',(3.2,-1.,4.3));
#5905=CARTESIAN_POINT('',(3.2,-1.16,4.3));
#5906=CARTESIAN_POINT('',(3.2,-1.,10.7));
#5907=CARTESIAN_POINT('',(3.2,-1.16,10.7));
#5908=CARTESIAN_POINT('',(0.,21.5,7.5));
#5909=CARTESIAN_POINT('',(-3.2,22.,4.3));
#5910=CARTESIAN_POINT('',(-3.2,22.16,4.3));
#5911=CARTESIAN_POINT('',(-3.2,22.,10.7));
#5912=CARTESIAN_POINT('',(-3.2,22.16,10.7));
#5913=CARTESIAN_POINT('',(3.2,22.,4.3));
#5914=CARTESIAN_POINT('',(3.2,22.16,4.3));
#5915=CARTESIAN_POINT('',(3.2,22.,10.7));
#5916=CARTESIAN_POINT('',(3.2,22.16,10.7));
#5917=CARTESIAN_POINT('',(0.,0.,0.));
#5918=CARTESIAN_POINT('',(0.,0.,0.));
#5919=CARTESIAN_POINT('Origin',(-0.2,27.,7.85));
#5920=CARTESIAN_POINT('',(-0.2,27.,8.06568542494924));
#5921=CARTESIAN_POINT('',(-0.2,29.,8.06568542494924));
#5922=CARTESIAN_POINT('',(-0.2,-3.5,8.06568542494924));
#5923=CARTESIAN_POINT('',(-0.2,27.,7.85));
#5924=CARTESIAN_POINT('',(-0.2,27.,8.2));
#5925=CARTESIAN_POINT('',(-0.2,29.,7.85));
#5926=CARTESIAN_POINT('',(-0.2,27.,7.85));
#5927=CARTESIAN_POINT('',(-0.2,29.,8.2));
#5928=CARTESIAN_POINT('Origin',(0.,29.,8.025));
#5929=CARTESIAN_POINT('',(0.2,29.,8.06568542494924));
#5930=CARTESIAN_POINT('Origin',(0.,29.,7.5));
#5931=CARTESIAN_POINT('',(0.2,29.,7.85));
#5932=CARTESIAN_POINT('',(-0.2,29.,7.85));
#5933=CARTESIAN_POINT('',(0.2,29.,7.85));
#5934=CARTESIAN_POINT('Origin',(0.2,27.,7.85));
#5935=CARTESIAN_POINT('',(0.2,27.,7.85));
#5936=CARTESIAN_POINT('',(-0.2,27.,7.85));
#5937=CARTESIAN_POINT('',(0.2,27.,7.85));
#5938=CARTESIAN_POINT('Origin',(0.2,27.,8.2));
#5939=CARTESIAN_POINT('',(0.2,27.,8.06568542494924));
#5940=CARTESIAN_POINT('',(0.2,-3.5,8.06568542494924));
#5941=CARTESIAN_POINT('',(0.2,27.,7.85));
#5942=CARTESIAN_POINT('Origin',(0.,27.,8.025));
#5943=CARTESIAN_POINT('Origin',(0.,27.,7.5));
#5944=CARTESIAN_POINT('Origin',(0.,-3.5,7.5));
#5945=CARTESIAN_POINT('',(-0.6,30.5,7.5));
#5946=CARTESIAN_POINT('Origin',(0.,30.5,7.5));
#5947=CARTESIAN_POINT('',(-0.6,-3.5,7.5));
#5948=CARTESIAN_POINT('',(-0.6,-3.5,7.5));
#5949=CARTESIAN_POINT('Origin',(0.,-3.5,7.5));
#5950=CARTESIAN_POINT('Origin',(0.,30.5,7.5));
#5951=CARTESIAN_POINT('Origin',(0.,-3.5,7.5));
#5952=CARTESIAN_POINT('',(0.,0.,0.));
#5953=CARTESIAN_POINT('',(0.,0.,0.));
#5954=CARTESIAN_POINT('Origin',(5.,4.8,0.));
#5955=CARTESIAN_POINT('',(3.8,4.8,-7.34788079488411E-17));
#5956=CARTESIAN_POINT('Origin',(4.4,4.8,0.));
#5957=CARTESIAN_POINT('Origin',(4.4,4.55,0.));
#5958=CARTESIAN_POINT('',(3.6,4.3,-9.79717439317882E-17));
#5959=CARTESIAN_POINT('Origin',(4.4,4.3,0.));
#5960=CARTESIAN_POINT('',(3.7,4.55,-8.57252759403146E-17));
#5961=CARTESIAN_POINT('Origin',(4.4,2.55,0.));
#5962=CARTESIAN_POINT('',(3.6,0.8,-9.79717439317882E-17));
#5963=CARTESIAN_POINT('Origin',(4.4,0.8,0.));
#5964=CARTESIAN_POINT('',(3.6,2.55,-9.79717439317882E-17));
#5965=CARTESIAN_POINT('Origin',(4.8,0.8,0.));
#5966=CARTESIAN_POINT('',(4.,0.8,-4.89858719658941E-17));
#5967=CARTESIAN_POINT('Origin',(4.4,0.8,0.));
#5968=CARTESIAN_POINT('Origin',(4.4,0.05,0.));
#5969=CARTESIAN_POINT('',(4.,-0.7,-4.89858719658941E-17));
#5970=CARTESIAN_POINT('Origin',(4.4,-0.7,0.));
#5971=CARTESIAN_POINT('',(4.,0.05,-4.89858719658941E-17));
#5972=CARTESIAN_POINT('Origin',(4.4,-0.7,0.));
#5973=CARTESIAN_POINT('Origin',(4.4,0.,0.));
#5974=CARTESIAN_POINT('',(4.38181818181818,-0.6,-0.399586563197017));
#5975=CARTESIAN_POINT('',(4.,-0.447213595499957,1.40845951270862E-17));
#5976=CARTESIAN_POINT('Ctrl Pts',(4.38181818181818,-0.6,-0.399586563197017));
#5977=CARTESIAN_POINT('Ctrl Pts',(4.37620354655216,-0.6,-0.399331088446446));
#5978=CARTESIAN_POINT('Ctrl Pts',(4.37059633849451,-0.599921176400794,-0.398957377684081));
#5979=CARTESIAN_POINT('Ctrl Pts',(4.35231513288062,-0.599405577873612,-0.397351597439964));
#5980=CARTESIAN_POINT('Ctrl Pts',(4.33972830709261,-0.598642847568908,-0.395635899495609));
#5981=CARTESIAN_POINT('Ctrl Pts',(4.31001303143016,-0.595878581860272,-0.390141553679429));
#5982=CARTESIAN_POINT('Ctrl Pts',(4.29310003081746,-0.593520874256089,-0.385840467860369));
#5983=CARTESIAN_POINT('Ctrl Pts',(4.24141718743348,-0.58396833212535,-0.369080440261527));
#5984=CARTESIAN_POINT('Ctrl Pts',(4.20867977226721,-0.574396002359473,-0.35308769317213));
#5985=CARTESIAN_POINT('Ctrl Pts',(4.13710416992423,-0.546662492416072,-0.305621410183058));
#5986=CARTESIAN_POINT('Ctrl Pts',(4.10145248427466,-0.526593672888128,-0.270643641048743));
#5987=CARTESIAN_POINT('Ctrl Pts',(4.04678809651788,-0.489398581579535,-0.193271805068502));
#5988=CARTESIAN_POINT('Ctrl Pts',(4.02636517822878,-0.471824419974506,-0.150618280859474));
#5989=CARTESIAN_POINT('Ctrl Pts',(4.00475562957405,-0.45203353900844,-0.0707222616040669));
#5990=CARTESIAN_POINT('Ctrl Pts',(4.,-0.447213595499957,-0.0358213625930324));
#5991=CARTESIAN_POINT('Ctrl Pts',(4.,-0.447213595499957,0.));
#5992=CARTESIAN_POINT('Ctrl Pts',(4.,-0.447213595499957,-4.2096619668615E-17));
#5993=CARTESIAN_POINT('Ctrl Pts',(4.,-0.447213595499957,0.00231828024966431));
#5994=CARTESIAN_POINT('Ctrl Pts',(4.00002015291119,-0.447233426516538,0.00464041591900193));
#5995=CARTESIAN_POINT('Ctrl Pts',(4.00078593665181,-0.447986619321796,0.0486042900487314));
#5996=CARTESIAN_POINT('Ctrl Pts',(4.00791128215643,-0.455206051708779,0.0886447085746181));
#5997=CARTESIAN_POINT('Ctrl Pts',(4.03587474981726,-0.479963706911242,0.172535559232532));
#5998=CARTESIAN_POINT('Ctrl Pts',(4.05952154543374,-0.499305325617665,0.215544140194275));
#5999=CARTESIAN_POINT('Ctrl Pts',(4.115931958945,-0.534538341716186,0.284471526737177));
#6000=CARTESIAN_POINT('Ctrl Pts',(4.14628233661512,-0.550362037136641,0.311973849714753));
#6001=CARTESIAN_POINT('Ctrl Pts',(4.21006393264307,-0.574803374422168,0.353766344633894));
#6002=CARTESIAN_POINT('Ctrl Pts',(4.24216830962295,-0.584104086647922,0.369319268652553));
#6003=CARTESIAN_POINT('Ctrl Pts',(4.29308262177289,-0.59351913040989,0.385837098757871));
#6004=CARTESIAN_POINT('Ctrl Pts',(4.31000257334402,-0.595876699074913,0.390138254734081));
#6005=CARTESIAN_POINT('Ctrl Pts',(4.33984346373323,-0.59865422370305,0.395658187711044));
#6006=CARTESIAN_POINT('Ctrl Pts',(4.35255940167626,-0.59942003186583,0.397384387659598));
#6007=CARTESIAN_POINT('Ctrl Pts',(4.37864659775072,-0.600140148714188,0.399652395423929));
#6008=CARTESIAN_POINT('Ctrl Pts',(4.39197122976054,-0.600060372790861,0.400141070011449));
#6009=CARTESIAN_POINT('Ctrl Pts',(4.42524642236728,-0.598768169203699,0.399701228150437));
#6010=CARTESIAN_POINT('Ctrl Pts',(4.44505102882446,-0.597014891071304,0.397946347201428));
#6011=CARTESIAN_POINT('Ctrl Pts',(4.51231374643158,-0.587907156256967,0.386945439318973));
#6012=CARTESIAN_POINT('Ctrl Pts',(4.55722896459207,-0.576234031361068,0.370738351126727));
#6013=CARTESIAN_POINT('Ctrl Pts',(4.64383263048066,-0.5452156510398,0.321498513032364));
#6014=CARTESIAN_POINT('Ctrl Pts',(4.68382910146734,-0.525117270017781,0.286611708354837));
#6015=CARTESIAN_POINT('Ctrl Pts',(4.74479838771145,-0.488962051837591,0.208211119095925));
#6016=CARTESIAN_POINT('Ctrl Pts',(4.76751221814709,-0.472539690182888,0.16532363822899));
#6017=CARTESIAN_POINT('Ctrl Pts',(4.793947837701,-0.45233115292012,0.0801450491942168));
#6018=CARTESIAN_POINT('Ctrl Pts',(4.80013660259258,-0.447101597189361,0.0399141590418927));
#6019=CARTESIAN_POINT('Ctrl Pts',(4.79985042703662,-0.447336228030294,-0.0451141645597526));
#6020=CARTESIAN_POINT('Ctrl Pts',(4.79259442840285,-0.453470503705387,-0.0875565986513605));
#6021=CARTESIAN_POINT('Ctrl Pts',(4.76254336881826,-0.476181588957065,-0.176742802554312));
#6022=CARTESIAN_POINT('Ctrl Pts',(4.73698137926376,-0.494272007313214,-0.221226370718438));
#6023=CARTESIAN_POINT('Ctrl Pts',(4.67589300813802,-0.528959279983926,-0.292989120825645));
#6024=CARTESIAN_POINT('Ctrl Pts',(4.64156068949428,-0.545654377209448,-0.321979194943134));
#6025=CARTESIAN_POINT('Ctrl Pts',(4.57349950221702,-0.570649410723138,-0.362013117337885));
#6026=CARTESIAN_POINT('Ctrl Pts',(4.54174415913774,-0.579993920599389,-0.375669546647045));
#6027=CARTESIAN_POINT('Ctrl Pts',(4.48184469738762,-0.59235489505887,-0.392487976854985));
#6028=CARTESIAN_POINT('Ctrl Pts',(4.45469661582122,-0.596251830509523,-0.397210764878501));
#6029=CARTESIAN_POINT('Ctrl Pts',(4.41199868606709,-0.599430494173245,-0.400104322948797));
#6030=CARTESIAN_POINT('Ctrl Pts',(4.3969025511922,-0.6,-0.40027292576925));
#6031=CARTESIAN_POINT('Ctrl Pts',(4.38181818181818,-0.6,-0.399586563197017));
#6032=CARTESIAN_POINT('',(4.,0.447213595499957,1.06151481751326E-17));
#6033=CARTESIAN_POINT('',(4.,0.,4.89858719658942E-17));
#6034=CARTESIAN_POINT('',(4.38181818181818,0.6,-0.399586563197017));
#6035=CARTESIAN_POINT('Ctrl Pts',(4.38181818181818,0.6,-0.399586563197017));
#6036=CARTESIAN_POINT('Ctrl Pts',(4.38217776987594,0.6,-0.399602925020183));
#6037=CARTESIAN_POINT('Ctrl Pts',(4.38253737948503,0.599999676740854,-0.399618801429084));
#6038=CARTESIAN_POINT('Ctrl Pts',(4.39810750269961,0.599971691179406,-0.400285149978334));
#6039=CARTESIAN_POINT('Ctrl Pts',(4.41335962542107,0.599365583135745,-0.400068337184671));
#6040=CARTESIAN_POINT('Ctrl Pts',(4.45609605239849,0.596076444344949,-0.39700592354558));
#6041=CARTESIAN_POINT('Ctrl Pts',(4.48315173565338,0.59213819454422,-0.392211691390051));
#6042=CARTESIAN_POINT('Ctrl Pts',(4.5562274106725,0.576906850691916,-0.371434861078584));
#6043=CARTESIAN_POINT('Ctrl Pts',(4.5994416592477,0.562448501081322,-0.349930526910355));
#6044=CARTESIAN_POINT('Ctrl Pts',(4.68197093066801,0.526887929791366,-0.289059421938731));
#6045=CARTESIAN_POINT('Ctrl Pts',(4.71927072326363,0.505032168549575,-0.247311177133964));
#6046=CARTESIAN_POINT('Ctrl Pts',(4.76835617637136,0.472224573632385,-0.161747869091691));
#6047=CARTESIAN_POINT('Ctrl Pts',(4.78412913104805,0.459943187027168,-0.120335510170092));
#6048=CARTESIAN_POINT('Ctrl Pts',(4.8004842088633,0.446911473500065,-0.0358681413616309));
#6049=CARTESIAN_POINT('Ctrl Pts',(4.80211129711387,0.445512317526093,0.00512209912648909));
#6050=CARTESIAN_POINT('Ctrl Pts',(4.79189040150874,0.45380427042988,0.0928053928501807));
#6051=CARTESIAN_POINT('Ctrl Pts',(4.77850571140352,0.464665209937273,0.136981831350341));
#6052=CARTESIAN_POINT('Ctrl Pts',(4.73651199214904,0.493999272271238,0.221864434033125));
#6053=CARTESIAN_POINT('Ctrl Pts',(4.70652254298001,0.512942829957004,0.261673250221586));
#6054=CARTESIAN_POINT('Ctrl Pts',(4.63981283945647,0.545961862488824,0.322778046340775));
#6055=CARTESIAN_POINT('Ctrl Pts',(4.60484752125829,0.560431345960551,0.346187806499183));
#6056=CARTESIAN_POINT('Ctrl Pts',(4.53107703569756,0.58280302533232,0.379877153356344));
#6057=CARTESIAN_POINT('Ctrl Pts',(4.49327004619306,0.591089762190358,0.391021773957148));
#6058=CARTESIAN_POINT('Ctrl Pts',(4.43565722321789,0.597872083748138,0.3988217367562));
#6059=CARTESIAN_POINT('Ctrl Pts',(4.41740282127395,0.599230533101231,0.400044418723135));
#6060=CARTESIAN_POINT('Ctrl Pts',(4.38605291211989,0.600123801224883,0.399966620420395));
#6061=CARTESIAN_POINT('Ctrl Pts',(4.37307485581441,0.600078055860439,0.399305346447973));
#6062=CARTESIAN_POINT('Ctrl Pts',(4.34707983335796,0.599129994834138,0.396700137951532));
#6063=CARTESIAN_POINT('Ctrl Pts',(4.3341144934305,0.598224910034854,0.394754522931063));
#6064=CARTESIAN_POINT('Ctrl Pts',(4.30271417169121,0.594971578276487,0.388449597781707));
#6065=CARTESIAN_POINT('Ctrl Pts',(4.28453727637576,0.592176175294015,0.383433197654118));
#6066=CARTESIAN_POINT('Ctrl Pts',(4.22586458639984,0.580243538593361,0.362717744715626));
#6067=CARTESIAN_POINT('Ctrl Pts',(4.18833529340542,0.567737042053699,0.341993684570505));
#6068=CARTESIAN_POINT('Ctrl Pts',(4.11283462612631,0.534171378857267,0.283547383735074));
#6069=CARTESIAN_POINT('Ctrl Pts',(4.07888753653551,0.51231402191844,0.243724831889356));
#6070=CARTESIAN_POINT('Ctrl Pts',(4.03269086728519,0.477679254985282,0.16387858814032));
#6071=CARTESIAN_POINT('Ctrl Pts',(4.01686967046718,0.463294474516269,0.123253857821745));
#6072=CARTESIAN_POINT('Ctrl Pts',(4.00269233005712,0.449913571793227,0.0534756547949087));
#6073=CARTESIAN_POINT('Ctrl Pts',(4.,0.447213595499957,0.0269126210022609));
#6074=CARTESIAN_POINT('Ctrl Pts',(4.,0.447213595499957,-2.77555756156289E-17));
#6075=CARTESIAN_POINT('Ctrl Pts',(4.,0.447213595499957,3.12250225675825E-17));
#6076=CARTESIAN_POINT('Ctrl Pts',(4.,0.447213595499957,-0.0109336371758505));
#6077=CARTESIAN_POINT('Ctrl Pts',(4.00044757096773,0.447655562220312,-0.0219249776368444));
#6078=CARTESIAN_POINT('Ctrl Pts',(4.00520900670299,0.452307037407336,-0.0794936286785903));
#6079=CARTESIAN_POINT('Ctrl Pts',(4.01683899054454,0.463589521272128,-0.121314660456946));
#6080=CARTESIAN_POINT('Ctrl Pts',(4.05044411504352,0.491640345747449,-0.199899424965473));
#6081=CARTESIAN_POINT('Ctrl Pts',(4.07632395532653,0.511152433757493,-0.239920550986411));
#6082=CARTESIAN_POINT('Ctrl Pts',(4.14319162351432,0.549072366528989,-0.310568720434486));
#6083=CARTESIAN_POINT('Ctrl Pts',(4.18393657245712,0.567086215733065,-0.340536354364695));
#6084=CARTESIAN_POINT('Ctrl Pts',(4.25308519475938,0.586109821373136,-0.372873616714749));
#6085=CARTESIAN_POINT('Ctrl Pts',(4.27683034868435,0.591075841926799,-0.381421283524454));
#6086=CARTESIAN_POINT('Ctrl Pts',(4.31562065419949,0.596457618518653,-0.391266435776889));
#6087=CARTESIAN_POINT('Ctrl Pts',(4.32991058664294,0.597905515290278,-0.394084038616911));
#6088=CARTESIAN_POINT('Ctrl Pts',(4.35677956565808,0.599605121795544,-0.397853848713028));
#6089=CARTESIAN_POINT('Ctrl Pts',(4.36925538216825,0.6,-0.399014936020011));
#6090=CARTESIAN_POINT('Ctrl Pts',(4.38181818181818,0.6,-0.399586563197017));
#6091=CARTESIAN_POINT('Origin',(-0.5,0.,0.));
#6092=CARTESIAN_POINT('',(-0.544630092356271,-2.77555756156289E-17,-0.25175));
#6093=CARTESIAN_POINT('',(-0.544630092356271,3.08304831685346E-17,0.25175));
#6094=CARTESIAN_POINT('Ctrl Pts',(-0.544630092356271,-2.77555756156289E-17,
-0.25175));
#6095=CARTESIAN_POINT('Ctrl Pts',(-0.544630092356271,-0.0320661161546808,
-0.25175));
#6096=CARTESIAN_POINT('Ctrl Pts',(-0.547762140631641,-0.0659494177282828,
-0.245259980626381));
#6097=CARTESIAN_POINT('Ctrl Pts',(-0.558600363408959,-0.127829426180881,
-0.219457148015658));
#6098=CARTESIAN_POINT('Ctrl Pts',(-0.566103947925634,-0.155868059910982,
-0.200160204416444));
#6099=CARTESIAN_POINT('Ctrl Pts',(-0.579856011772299,-0.200132614131413,
-0.155895650196014));
#6100=CARTESIAN_POINT('Ctrl Pts',(-0.587059973454843,-0.219450369823919,
-0.127846763396003));
#6101=CARTESIAN_POINT('Ctrl Pts',(-0.597191733030102,-0.245269281484808,
-0.0659260305857526));
#6102=CARTESIAN_POINT('Ctrl Pts',(-0.6,-0.25175,-0.0320261671617185));
#6103=CARTESIAN_POINT('Ctrl Pts',(-0.6,-0.25175,0.0320261671617186));
#6104=CARTESIAN_POINT('Ctrl Pts',(-0.597191733030102,-0.245269281484808,
0.0659260305857528));
#6105=CARTESIAN_POINT('Ctrl Pts',(-0.587059973454843,-0.219450369823919,
0.127846763396003));
#6106=CARTESIAN_POINT('Ctrl Pts',(-0.579856011772299,-0.200132614131413,
0.155895650196014));
#6107=CARTESIAN_POINT('Ctrl Pts',(-0.566103947925634,-0.155868059910982,
0.200160204416444));
#6108=CARTESIAN_POINT('Ctrl Pts',(-0.558600363408959,-0.127829426180881,
0.219457148015658));
#6109=CARTESIAN_POINT('Ctrl Pts',(-0.547762140631641,-0.0659494177282828,
0.245259980626381));
#6110=CARTESIAN_POINT('Ctrl Pts',(-0.544630092356271,-0.0320661161546807,
0.25175));
#6111=CARTESIAN_POINT('Ctrl Pts',(-0.544630092356271,0.,0.25175));
#6112=CARTESIAN_POINT('Ctrl Pts',(-0.544630092356271,2.08166817117217E-17,
0.25175));
#6113=CARTESIAN_POINT('Ctrl Pts',(-0.544630092356271,0.0320661161546808,
0.25175));
#6114=CARTESIAN_POINT('Ctrl Pts',(-0.547762140631641,0.0659494177282828,
0.245259980626381));
#6115=CARTESIAN_POINT('Ctrl Pts',(-0.558600363408959,0.127829426180881,
0.219457148015658));
#6116=CARTESIAN_POINT('Ctrl Pts',(-0.566103947925634,0.155868059910982,
0.200160204416444));
#6117=CARTESIAN_POINT('Ctrl Pts',(-0.579856011772299,0.200132614131413,
0.155895650196014));
#6118=CARTESIAN_POINT('Ctrl Pts',(-0.587059973454843,0.219450369823919,
0.127846763396003));
#6119=CARTESIAN_POINT('Ctrl Pts',(-0.597191733030102,0.245269281484808,
0.0659260305857527));
#6120=CARTESIAN_POINT('Ctrl Pts',(-0.6,0.25175,0.0320261671617186));
#6121=CARTESIAN_POINT('Ctrl Pts',(-0.6,0.25175,-0.0320261671617186));
#6122=CARTESIAN_POINT('Ctrl Pts',(-0.597191733030102,0.245269281484808,
-0.0659260305857527));
#6123=CARTESIAN_POINT('Ctrl Pts',(-0.587059973454843,0.219450369823919,
-0.127846763396003));
#6124=CARTESIAN_POINT('Ctrl Pts',(-0.579856011772299,0.200132614131413,
-0.155895650196014));
#6125=CARTESIAN_POINT('Ctrl Pts',(-0.566103947925634,0.155868059910982,
-0.200160204416444));
#6126=CARTESIAN_POINT('Ctrl Pts',(-0.558600363408959,0.127829426180881,
-0.219457148015658));
#6127=CARTESIAN_POINT('Ctrl Pts',(-0.547762140631641,0.0659494177282829,
-0.245259980626381));
#6128=CARTESIAN_POINT('Ctrl Pts',(-0.544630092356271,0.0320661161546808,
-0.25175));
#6129=CARTESIAN_POINT('Ctrl Pts',(-0.544630092356271,1.38777878078145E-17,
-0.25175));
#6130=CARTESIAN_POINT('',(-1.58007023182516,1.88846885362209E-17,0.25175));
#6131=CARTESIAN_POINT('',(-0.5,3.08304831685346E-17,0.25175));
#6132=CARTESIAN_POINT('',(-1.6,0.25175,-8.06245091720202E-17));
#6133=CARTESIAN_POINT('Ctrl Pts',(-1.6,0.25175,3.46944695195361E-17));
#6134=CARTESIAN_POINT('Ctrl Pts',(-1.6,0.25175,0.0316665562812107));
#6135=CARTESIAN_POINT('Ctrl Pts',(-1.59896422950043,0.245410672078977,0.0654081672606842));
#6136=CARTESIAN_POINT('Ctrl Pts',(-1.59522075716076,0.219702194881036,0.127418882159871));
#6137=CARTESIAN_POINT('Ctrl Pts',(-1.59256535387617,0.200335934524935,0.155692329802492));
#6138=CARTESIAN_POINT('Ctrl Pts',(-1.58756727523672,0.155691857576545,0.200336406750882));
#6139=CARTESIAN_POINT('Ctrl Pts',(-1.58489737644125,0.12741861324567,0.219702296671568));
#6140=CARTESIAN_POINT('Ctrl Pts',(-1.58112064026101,0.0654085945942507,
0.245410504610724));
#6141=CARTESIAN_POINT('Ctrl Pts',(-1.58007023182516,0.0316672261988669,
0.25175));
#6142=CARTESIAN_POINT('Ctrl Pts',(-1.58007023182516,-6.93889390390723E-18,
0.25175));
#6143=CARTESIAN_POINT('',(-1.58007023182516,0.,-0.25175));
#6144=CARTESIAN_POINT('Ctrl Pts',(-1.58007023182516,0.,-0.25175));
#6145=CARTESIAN_POINT('Ctrl Pts',(-1.58007023182516,0.0316672261988669,
-0.25175));
#6146=CARTESIAN_POINT('Ctrl Pts',(-1.58112064026101,0.0654085945942508,
-0.245410504610724));
#6147=CARTESIAN_POINT('Ctrl Pts',(-1.58489737644125,0.12741861324567,-0.219702296671568));
#6148=CARTESIAN_POINT('Ctrl Pts',(-1.58756727523672,0.155691857576545,-0.200336406750882));
#6149=CARTESIAN_POINT('Ctrl Pts',(-1.59256535387617,0.200335934524935,-0.155692329802492));
#6150=CARTESIAN_POINT('Ctrl Pts',(-1.59522075716076,0.219702194881036,-0.127418882159871));
#6151=CARTESIAN_POINT('Ctrl Pts',(-1.59896422950043,0.245410672078977,-0.0654081672606842));
#6152=CARTESIAN_POINT('Ctrl Pts',(-1.6,0.25175,-0.0316665562812106));
#6153=CARTESIAN_POINT('Ctrl Pts',(-1.6,0.25175,4.16333634234434E-17));
#6154=CARTESIAN_POINT('',(-1.6,-0.25175,-1.01441190883742E-16));
#6155=CARTESIAN_POINT('Ctrl Pts',(-1.6,-0.25175,-6.93889390390723E-18));
#6156=CARTESIAN_POINT('Ctrl Pts',(-1.6,-0.25175,-0.0316665562812106));
#6157=CARTESIAN_POINT('Ctrl Pts',(-1.59896422950043,-0.245410672078977,
-0.0654081672606842));
#6158=CARTESIAN_POINT('Ctrl Pts',(-1.59522075716076,-0.219702194881036,
-0.127418882159871));
#6159=CARTESIAN_POINT('Ctrl Pts',(-1.59256535387617,-0.200335934524935,
-0.155692329802492));
#6160=CARTESIAN_POINT('Ctrl Pts',(-1.58756727523672,-0.155691857576545,
-0.200336406750882));
#6161=CARTESIAN_POINT('Ctrl Pts',(-1.58489737644125,-0.12741861324567,-0.219702296671568));
#6162=CARTESIAN_POINT('Ctrl Pts',(-1.58112064026101,-0.0654085945942508,
-0.245410504610724));
#6163=CARTESIAN_POINT('Ctrl Pts',(-1.58007023182516,-0.0316672261988669,
-0.25175));
#6164=CARTESIAN_POINT('Ctrl Pts',(-1.58007023182516,0.,-0.25175));
#6165=CARTESIAN_POINT('Ctrl Pts',(-1.58007023182516,-6.93889390390723E-18,
0.25175));
#6166=CARTESIAN_POINT('Ctrl Pts',(-1.58007023182516,-0.0316672261988669,
0.25175));
#6167=CARTESIAN_POINT('Ctrl Pts',(-1.58112064026101,-0.0654085945942507,
0.245410504610724));
#6168=CARTESIAN_POINT('Ctrl Pts',(-1.58489737644125,-0.12741861324567,0.219702296671568));
#6169=CARTESIAN_POINT('Ctrl Pts',(-1.58756727523672,-0.155691857576545,
0.200336406750882));
#6170=CARTESIAN_POINT('Ctrl Pts',(-1.59256535387617,-0.200335934524935,
0.155692329802492));
#6171=CARTESIAN_POINT('Ctrl Pts',(-1.59522075716076,-0.219702194881036,
0.127418882159871));
#6172=CARTESIAN_POINT('Ctrl Pts',(-1.59896422950043,-0.245410672078977,
0.0654081672606843));
#6173=CARTESIAN_POINT('Ctrl Pts',(-1.6,-0.25175,0.0316665562812106));
#6174=CARTESIAN_POINT('Ctrl Pts',(-1.6,-0.25175,0.));
#6175=CARTESIAN_POINT('Origin',(-0.2,0.,0.55));
#6176=CARTESIAN_POINT('',(-0.2,1.9,0.78));
#6177=CARTESIAN_POINT('',(-0.2,1.9,0.565685424949238));
#6178=CARTESIAN_POINT('',(-0.2,1.9,0.275));
#6179=CARTESIAN_POINT('',(-0.2,-1.9,0.78));
#6180=CARTESIAN_POINT('',(-0.2,0.,0.78));
#6181=CARTESIAN_POINT('',(-0.2,-1.9,0.565685424949238));
#6182=CARTESIAN_POINT('',(-0.2,-1.9,0.275));
#6183=CARTESIAN_POINT('',(-0.2,0.,0.565685424949238));
#6184=CARTESIAN_POINT('Origin',(0.2,0.,0.78));
#6185=CARTESIAN_POINT('',(0.2,1.9,0.565685424949238));
#6186=CARTESIAN_POINT('',(0.2,1.9,0.78));
#6187=CARTESIAN_POINT('',(0.2,1.9,0.39));
#6188=CARTESIAN_POINT('',(0.2,-1.9,0.565685424949238));
#6189=CARTESIAN_POINT('',(0.2,0.,0.565685424949238));
#6190=CARTESIAN_POINT('',(0.2,-1.9,0.78));
#6191=CARTESIAN_POINT('',(0.2,-1.9,0.39));
#6192=CARTESIAN_POINT('',(0.2,0.,0.78));
#6193=CARTESIAN_POINT('Origin',(-0.2,0.,0.78));
#6194=CARTESIAN_POINT('',(0.7,1.9,0.78));
#6195=CARTESIAN_POINT('',(0.2,-1.9,0.78));
#6196=CARTESIAN_POINT('Origin',(0.6,-1.9,0.));
#6197=CARTESIAN_POINT('',(-1.6,-1.9,-1.95943487863577E-16));
#6198=CARTESIAN_POINT('Origin',(0.,-1.9,0.));
#6199=CARTESIAN_POINT('Origin',(0.,-1.9,0.));
#6200=CARTESIAN_POINT('Origin',(0.,0.,0.));
#6201=CARTESIAN_POINT('Origin',(0.,1.9,0.));
#6202=CARTESIAN_POINT('Origin',(-0.700000000000001,0.,1.21243556529821));
#6203=CARTESIAN_POINT('',(-1.97639320225002,-0.4,3.42321344203079));
#6204=CARTESIAN_POINT('',(-1.54303420125535,4.36782978783278E-17,3.47261363439071));
#6205=CARTESIAN_POINT('Ctrl Pts',(-1.97639320225002,-0.4,3.42321344203079));
#6206=CARTESIAN_POINT('Ctrl Pts',(-1.95415831773611,-0.4,3.4360507585903));
#6207=CARTESIAN_POINT('Ctrl Pts',(-1.9310257528573,-0.397543666260907,3.44654300794432));
#6208=CARTESIAN_POINT('Ctrl Pts',(-1.87011275937252,-0.385296442875872,
3.46805551377425));
#6209=CARTESIAN_POINT('Ctrl Pts',(-1.83255059885217,-0.372362902338019,
3.47567016958921));
#6210=CARTESIAN_POINT('Ctrl Pts',(-1.74343033527116,-0.329622538051278,
3.48635323641216));
#6211=CARTESIAN_POINT('Ctrl Pts',(-1.69170226994963,-0.293529822220925,
3.48570386152998));
#6212=CARTESIAN_POINT('Ctrl Pts',(-1.61564653912222,-0.213132057516649,
3.4812739628721));
#6213=CARTESIAN_POINT('Ctrl Pts',(-1.58806423417247,-0.172744633626715,
3.4782529204836));
#6214=CARTESIAN_POINT('Ctrl Pts',(-1.55315160595641,-0.0896107157758499,
3.47405876016096));
#6215=CARTESIAN_POINT('Ctrl Pts',(-1.5440326911925,-0.048847909102319,3.47275072127476));
#6216=CARTESIAN_POINT('Ctrl Pts',(-1.54305991676911,-0.00467961343368063,
3.47261716680632));
#6217=CARTESIAN_POINT('Ctrl Pts',(-1.54303420125535,-0.00233835250145938,
3.47261363439071));
#6218=CARTESIAN_POINT('Ctrl Pts',(-1.54303420125535,1.04859257011983E-17,
3.47261363439071));
#6219=CARTESIAN_POINT('',(-2.2358545242829,-2.10234890309935E-17,3.07261363439071));
#6220=CARTESIAN_POINT('Ctrl Pts',(-2.2358545242829,-2.08166817117217E-17,
3.07261363439071));
#6221=CARTESIAN_POINT('Ctrl Pts',(-2.2358545242829,-0.0383517947844003,
3.07261363439071));
#6222=CARTESIAN_POINT('Ctrl Pts',(-2.23325695879738,-0.0760113765503611,
3.0790942798427));
#6223=CARTESIAN_POINT('Ctrl Pts',(-2.22115055352356,-0.160957090841631,
3.10774035695596));
#6224=CARTESIAN_POINT('Ctrl Pts',(-2.20980404970244,-0.205137357634188,
3.134001114773));
#6225=CARTESIAN_POINT('Ctrl Pts',(-2.17521580468705,-0.28961400567012,3.20357758115091));
#6226=CARTESIAN_POINT('Ctrl Pts',(-2.15015969108582,-0.326524134432438,
3.24882900544019));
#6227=CARTESIAN_POINT('Ctrl Pts',(-2.09653256150325,-0.370775784308148,
3.32158936294835));
#6228=CARTESIAN_POINT('Ctrl Pts',(-2.07090576981203,-0.384320524321436,
3.35106094569693));
#6229=CARTESIAN_POINT('Ctrl Pts',(-2.02085331447703,-0.397355586307629,
3.39445851101291));
#6230=CARTESIAN_POINT('Ctrl Pts',(-1.99946741642565,-0.4,3.40989153826515));
#6231=CARTESIAN_POINT('Ctrl Pts',(-1.97639320225002,-0.4,3.42321344203079));
#6232=CARTESIAN_POINT('',(-1.12100683075526,0.,1.14164078649987));
#6233=CARTESIAN_POINT('',(-1.04641016151378,-4.89858719658941E-17,1.01243556529821));
#6234=CARTESIAN_POINT('Ctrl Pts',(-1.12100683075526,0.,1.14164078649987));
#6235=CARTESIAN_POINT('Ctrl Pts',(-1.12100683075526,0.0504597642713565,
1.14164078649987));
#6236=CARTESIAN_POINT('Ctrl Pts',(-1.11359645548276,0.1041286832042,1.1490623967528));
#6237=CARTESIAN_POINT('Ctrl Pts',(-1.08303934555689,0.202612274012173,1.17790798500778));
#6238=CARTESIAN_POINT('Ctrl Pts',(-1.05982504365452,0.247446581818911,1.19919313648287));
#6239=CARTESIAN_POINT('Ctrl Pts',(-1.00487832123842,0.318233894120626,1.24559724615223));
#6240=CARTESIAN_POINT('Ctrl Pts',(-0.969414884906718,0.348984503722909,
1.27384551059033));
#6241=CARTESIAN_POINT('Ctrl Pts',(-0.888861576521062,0.389873348412022,
1.33130488677705));
#6242=CARTESIAN_POINT('Ctrl Pts',(-0.843693327768004,0.4,1.36041429150645));
#6243=CARTESIAN_POINT('Ctrl Pts',(-0.756306672231997,0.4,1.41086700060375));
#6244=CARTESIAN_POINT('Ctrl Pts',(-0.708513063870764,0.389873348412022,
1.43542914910365));
#6245=CARTESIAN_POINT('Ctrl Pts',(-0.618475130214631,0.348984503722909,
1.47646067243115));
#6246=CARTESIAN_POINT('Ctrl Pts',(-0.576279697432564,0.318233894120626,
1.49304877698084));
#6247=CARTESIAN_POINT('Ctrl Pts',(-0.508619198410849,0.247446581818911,
1.5174319796132));
#6248=CARTESIAN_POINT('Ctrl Pts',(-0.478578565558828,0.202612274012173,
1.52689357905423));
#6249=CARTESIAN_POINT('Ctrl Pts',(-0.438318998379975,0.1041286832042,1.53893401838878));
#6250=CARTESIAN_POINT('Ctrl Pts',(-0.428186507727709,0.0504597642713565,
1.54164078649987));
#6251=CARTESIAN_POINT('Ctrl Pts',(-0.428186507727709,-0.0504597642713564,
1.54164078649987));
#6252=CARTESIAN_POINT('Ctrl Pts',(-0.438318998379975,-0.1041286832042,1.53893401838878));
#6253=CARTESIAN_POINT('Ctrl Pts',(-0.478578565558828,-0.202612274012173,
1.52689357905423));
#6254=CARTESIAN_POINT('Ctrl Pts',(-0.508619198410849,-0.247446581818911,
1.5174319796132));
#6255=CARTESIAN_POINT('Ctrl Pts',(-0.576279697432564,-0.318233894120626,
1.49304877698084));
#6256=CARTESIAN_POINT('Ctrl Pts',(-0.618475130214631,-0.348984503722909,
1.47646067243115));
#6257=CARTESIAN_POINT('Ctrl Pts',(-0.708513063870764,-0.389873348412022,
1.43542914910365));
#6258=CARTESIAN_POINT('Ctrl Pts',(-0.756306672231997,-0.4,1.41086700060375));
#6259=CARTESIAN_POINT('Ctrl Pts',(-0.843693327768004,-0.4,1.36041429150645));
#6260=CARTESIAN_POINT('Ctrl Pts',(-0.888861576521062,-0.389873348412022,
1.33130488677705));
#6261=CARTESIAN_POINT('Ctrl Pts',(-0.969414884906718,-0.348984503722909,
1.27384551059033));
#6262=CARTESIAN_POINT('Ctrl Pts',(-1.00487832123842,-0.318233894120626,
1.24559724615223));
#6263=CARTESIAN_POINT('Ctrl Pts',(-1.05982504365452,-0.247446581818911,
1.19919313648287));
#6264=CARTESIAN_POINT('Ctrl Pts',(-1.08303934555689,-0.202612274012173,
1.17790798500778));
#6265=CARTESIAN_POINT('Ctrl Pts',(-1.11359645548276,-0.1041286832042,1.1490623967528));
#6266=CARTESIAN_POINT('Ctrl Pts',(-1.12100683075526,-0.0504597642713565,
1.14164078649987));
#6267=CARTESIAN_POINT('Ctrl Pts',(-1.12100683075526,-1.38777878078145E-17,
1.14164078649987));
#6268=CARTESIAN_POINT('Ctrl Pts',(-1.54303420125535,6.24500451351651E-17,
3.47261363439071));
#6269=CARTESIAN_POINT('Ctrl Pts',(-1.54303420125535,0.0410730673371918,
3.47261363439071));
#6270=CARTESIAN_POINT('Ctrl Pts',(-1.55095885731966,0.0812488103419988,
3.47375555118006));
#6271=CARTESIAN_POINT('Ctrl Pts',(-1.58495764629444,0.168643605332508,3.47792115802208));
#6272=CARTESIAN_POINT('Ctrl Pts',(-1.61486601851427,0.212871126833583,3.48130423813646));
#6273=CARTESIAN_POINT('Ctrl Pts',(-1.68826827178664,0.289288653612537,3.48542183788627));
#6274=CARTESIAN_POINT('Ctrl Pts',(-1.73220819761744,0.321562705912147,3.4861545786764));
#6275=CARTESIAN_POINT('Ctrl Pts',(-1.81695233056502,0.366289871498909,3.47834349980413));
#6276=CARTESIAN_POINT('Ctrl Pts',(-1.8573504302408,0.38158281389927,3.47138302834526));
#6277=CARTESIAN_POINT('Ctrl Pts',(-1.92264474793187,0.396376989861723,3.45003490626818));
#6278=CARTESIAN_POINT('Ctrl Pts',(-1.94731404531759,0.399534030132352,3.43946670387874));
#6279=CARTESIAN_POINT('Ctrl Pts',(-1.99398984114484,0.400357587283029,3.4134650277082));
#6280=CARTESIAN_POINT('Ctrl Pts',(-2.01531311918225,0.398184081632147,3.3986128265759));
#6281=CARTESIAN_POINT('Ctrl Pts',(-2.06441253258454,0.386733579315055,3.35745440071872));
#6282=CARTESIAN_POINT('Ctrl Pts',(-2.08944120109624,0.37471741504947,3.32984347089212));
#6283=CARTESIAN_POINT('Ctrl Pts',(-2.1435825547406,0.334141370748261,3.25932472726254));
#6284=CARTESIAN_POINT('Ctrl Pts',(-2.16934579305907,0.299193471253548,3.21427723761843));
#6285=CARTESIAN_POINT('Ctrl Pts',(-2.20475499729868,0.22024819873023,3.14480978899578));
#6286=CARTESIAN_POINT('Ctrl Pts',(-2.21652694497689,0.17986122270608,3.11828750797817));
#6287=CARTESIAN_POINT('Ctrl Pts',(-2.23122850773119,0.0967734525439114,
3.08409367525424));
#6288=CARTESIAN_POINT('Ctrl Pts',(-2.23502289292351,0.0560978356893851,
3.07465248016042));
#6289=CARTESIAN_POINT('Ctrl Pts',(-2.23581459500602,0.00945212461835248,
3.07271160407144));
#6290=CARTESIAN_POINT('Ctrl Pts',(-2.2358545242829,0.00472081811281322,
3.07261363439071));
#6291=CARTESIAN_POINT('Ctrl Pts',(-2.2358545242829,-6.29346629103429E-18,
3.07261363439071));
#6292=CARTESIAN_POINT('Origin',(-0.7,0.,-1.21243556529821));
#6293=CARTESIAN_POINT('',(-1.97639320225002,-0.4,-3.42321344203079));
#6294=CARTESIAN_POINT('',(-2.23585452428289,1.93921692146525E-17,-3.07261363439072));
#6295=CARTESIAN_POINT('Ctrl Pts',(-1.97639320225002,-0.4,-3.42321344203079));
#6296=CARTESIAN_POINT('Ctrl Pts',(-1.99862808676393,-0.4,-3.41037612547128));
#6297=CARTESIAN_POINT('Ctrl Pts',(-2.01928092368676,-0.397543666260908,
-3.39558886130855));
#6298=CARTESIAN_POINT('Ctrl Pts',(-2.06836779697694,-0.385296442875871,
-3.35359291444514));
#6299=CARTESIAN_POINT('Ctrl Pts',(-2.09374336261395,-0.372362902338017,
-3.32487045712097));
#6300=CARTESIAN_POINT('Ctrl Pts',(-2.14755530166345,-0.32962253805128,-3.25303157827933));
#6301=CARTESIAN_POINT('Ctrl Pts',(-2.17285695917966,-0.29352982222093,-3.20790907218117));
#6302=CARTESIAN_POINT('Ctrl Pts',(-2.20704841981946,-0.213132057516642,
-3.1398279278523));
#6303=CARTESIAN_POINT('Ctrl Pts',(-2.21822327283998,-0.172744633626709,
-3.11443042987664));
#6304=CARTESIAN_POINT('Ctrl Pts',(-2.23204733756106,-0.0896107157758442,
-3.08209812676733));
#6305=CARTESIAN_POINT('Ctrl Pts',(-2.23547400003843,-0.0488479091023135,
-3.07354689548374));
#6306=CARTESIAN_POINT('Ctrl Pts',(-2.23584472568767,-0.00467961343367746,
-3.07263767088671));
#6307=CARTESIAN_POINT('Ctrl Pts',(-2.23585452428289,-0.00233835250145779,
-3.07261363439072));
#6308=CARTESIAN_POINT('Ctrl Pts',(-2.23585452428289,1.78666159054142E-17,
-3.07261363439072));
#6309=CARTESIAN_POINT('',(-1.54303420125534,-1.06151481751326E-17,-3.47261363439072));
#6310=CARTESIAN_POINT('Ctrl Pts',(-1.54303420125534,-2.77555756156289E-17,
-3.47261363439072));
#6311=CARTESIAN_POINT('Ctrl Pts',(-1.54303420125534,-0.0383517947843985,
-3.47261363439072));
#6312=CARTESIAN_POINT('Ctrl Pts',(-1.54994538759244,-0.0760113765503578,
-3.47360439941826));
#6313=CARTESIAN_POINT('Ctrl Pts',(-1.5808068207282,-0.160957090841637,-3.47744298345925));
#6314=CARTESIAN_POINT('Ctrl Pts',(-1.60922255603095,-0.205137357634195,
-3.48074700181454));
#6315=CARTESIAN_POINT('Ctrl Pts',(-1.68677166592746,-0.289614005670115,
-3.48558093614785));
#6316=CARTESIAN_POINT('Ctrl Pts',(-1.73848860572002,-0.326524134432436,
-3.48650741739372));
#6317=CARTESIAN_POINT('Ctrl Pts',(-1.82831448850183,-0.370775784308151,
-3.47644513959724));
#6318=CARTESIAN_POINT('Ctrl Pts',(-1.86665102369743,-0.384320524321437,
-3.46898747834945));
#6319=CARTESIAN_POINT('Ctrl Pts',(-1.92926064539097,-0.397355586307629,
-3.44733956316554));
#6320=CARTESIAN_POINT('Ctrl Pts',(-1.95331898807439,-0.4,-3.43653534579643));
#6321=CARTESIAN_POINT('Ctrl Pts',(-1.97639320225002,-0.4,-3.42321344203079));
#6322=CARTESIAN_POINT('',(-0.428186507727708,-2.77555756156289E-17,-1.54164078649987));
#6323=CARTESIAN_POINT('',(-0.353589838486224,-4.89858719658941E-17,-1.41243556529821));
#6324=CARTESIAN_POINT('Ctrl Pts',(-0.428186507727708,-2.77555756156289E-17,
-1.54164078649987));
#6325=CARTESIAN_POINT('Ctrl Pts',(-0.428186507727708,0.0504597642713564,
-1.54164078649987));
#6326=CARTESIAN_POINT('Ctrl Pts',(-0.438318998379974,0.1041286832042,-1.53893401838878));
#6327=CARTESIAN_POINT('Ctrl Pts',(-0.478578565558827,0.202612274012173,
-1.52689357905423));
#6328=CARTESIAN_POINT('Ctrl Pts',(-0.508619198410847,0.247446581818911,
-1.5174319796132));
#6329=CARTESIAN_POINT('Ctrl Pts',(-0.576279697432563,0.318233894120627,
-1.49304877698084));
#6330=CARTESIAN_POINT('Ctrl Pts',(-0.61847513021463,0.348984503722909,-1.47646067243115));
#6331=CARTESIAN_POINT('Ctrl Pts',(-0.708513063870763,0.389873348412022,
-1.43542914910365));
#6332=CARTESIAN_POINT('Ctrl Pts',(-0.756306672231996,0.4,-1.41086700060375));
#6333=CARTESIAN_POINT('Ctrl Pts',(-0.843693327768003,0.4,-1.36041429150645));
#6334=CARTESIAN_POINT('Ctrl Pts',(-0.888861576521061,0.389873348412022,
-1.33130488677705));
#6335=CARTESIAN_POINT('Ctrl Pts',(-0.969414884906717,0.348984503722909,
-1.27384551059033));
#6336=CARTESIAN_POINT('Ctrl Pts',(-1.00487832123841,0.318233894120626,-1.24559724615223));
#6337=CARTESIAN_POINT('Ctrl Pts',(-1.05982504365452,0.247446581818911,-1.19919313648287));
#6338=CARTESIAN_POINT('Ctrl Pts',(-1.08303934555689,0.202612274012173,-1.17790798500778));
#6339=CARTESIAN_POINT('Ctrl Pts',(-1.11359645548276,0.1041286832042,-1.1490623967528));
#6340=CARTESIAN_POINT('Ctrl Pts',(-1.12100683075526,0.0504597642713564,
-1.14164078649987));
#6341=CARTESIAN_POINT('Ctrl Pts',(-1.12100683075526,-0.0504597642713564,
-1.14164078649987));
#6342=CARTESIAN_POINT('Ctrl Pts',(-1.11359645548276,-0.1041286832042,-1.1490623967528));
#6343=CARTESIAN_POINT('Ctrl Pts',(-1.08303934555689,-0.202612274012173,
-1.17790798500778));
#6344=CARTESIAN_POINT('Ctrl Pts',(-1.05982504365452,-0.247446581818911,
-1.19919313648287));
#6345=CARTESIAN_POINT('Ctrl Pts',(-1.00487832123841,-0.318233894120626,
-1.24559724615223));
#6346=CARTESIAN_POINT('Ctrl Pts',(-0.969414884906717,-0.348984503722909,
-1.27384551059034));
#6347=CARTESIAN_POINT('Ctrl Pts',(-0.888861576521061,-0.389873348412022,
-1.33130488677705));
#6348=CARTESIAN_POINT('Ctrl Pts',(-0.843693327768003,-0.4,-1.36041429150645));
#6349=CARTESIAN_POINT('Ctrl Pts',(-0.756306672231996,-0.4,-1.41086700060375));
#6350=CARTESIAN_POINT('Ctrl Pts',(-0.708513063870763,-0.389873348412022,
-1.43542914910365));
#6351=CARTESIAN_POINT('Ctrl Pts',(-0.61847513021463,-0.348984503722909,
-1.47646067243115));
#6352=CARTESIAN_POINT('Ctrl Pts',(-0.576279697432563,-0.318233894120627,
-1.49304877698084));
#6353=CARTESIAN_POINT('Ctrl Pts',(-0.508619198410847,-0.247446581818911,
-1.5174319796132));
#6354=CARTESIAN_POINT('Ctrl Pts',(-0.478578565558827,-0.202612274012173,
-1.52689357905423));
#6355=CARTESIAN_POINT('Ctrl Pts',(-0.438318998379974,-0.1041286832042,-1.53893401838878));
#6356=CARTESIAN_POINT('Ctrl Pts',(-0.428186507727708,-0.0504597642713564,
-1.54164078649987));
#6357=CARTESIAN_POINT('Ctrl Pts',(-0.428186507727708,0.,-1.54164078649987));
#6358=CARTESIAN_POINT('Ctrl Pts',(-2.23585452428289,7.63278329429795E-17,
-3.07261363439072));
#6359=CARTESIAN_POINT('Ctrl Pts',(-2.23585452428289,0.0410730673371933,
-3.07261363439072));
#6360=CARTESIAN_POINT('Ctrl Pts',(-2.23288112519932,0.0812488103420015,
-3.08004754625334));
#6361=CARTESIAN_POINT('Ctrl Pts',(-2.2194892520593,0.168643605332515,-3.11157416462442));
#6362=CARTESIAN_POINT('Ctrl Pts',(-2.20746489927147,0.212871126833592,-3.13916711480983));
#6363=CARTESIAN_POINT('Ctrl Pts',(-2.17432971862124,0.289288653612542,-3.20479413071362));
#6364=CARTESIAN_POINT('Ctrl Pts',(-2.15299432784447,0.321562705912151,-3.24321359311856));
#6365=CARTESIAN_POINT('Ctrl Pts',(-2.10385766863634,0.366289871498909,-3.31269862563671));
#6366=CARTESIAN_POINT('Ctrl Pts',(-2.07763067369275,0.381582813899271,-3.34420417049112));
#6367=CARTESIAN_POINT('Ctrl Pts',(-2.02649549880538,0.396376989861723,-3.39007664729581));
#6368=CARTESIAN_POINT('Ctrl Pts',(-2.00500851837093,0.399534030132352,-3.40615678433065));
#6369=CARTESIAN_POINT('Ctrl Pts',(-1.95915250835263,0.400357587283029,-3.43357837117363));
#6370=CARTESIAN_POINT('Ctrl Pts',(-1.93562848585123,0.398184081632146,-3.44461877107984));
#6371=CARTESIAN_POINT('Ctrl Pts',(-1.875434536778,0.386733579315055,-3.46656089746854));
#6372=CARTESIAN_POINT('Ctrl Pts',(-1.83900843587021,0.374717415049472,-3.47443089530928));
#6373=CARTESIAN_POINT('Ctrl Pts',(-1.75086673562183,0.334141370748251,-3.48605931114578));
#6374=CARTESIAN_POINT('Ctrl Pts',(-1.69897284605408,0.29919347125353,-3.48584718519127));
#6375=CARTESIAN_POINT('Ctrl Pts',(-1.62110766869098,0.220248198730226,-3.48177873127923));
#6376=CARTESIAN_POINT('Ctrl Pts',(-1.59225272572432,0.179861222706076,-3.47871239651179));
#6377=CARTESIAN_POINT('Ctrl Pts',(-1.55528921655549,0.0967734525439036,
-3.47434740697038));
#6378=CARTESIAN_POINT('Ctrl Pts',(-1.545215709166,0.0560978356893791,-3.47291284339176));
#6379=CARTESIAN_POINT('Ctrl Pts',(-1.54313901012609,0.00945212461834998,
-3.47262803946294));
#6380=CARTESIAN_POINT('Ctrl Pts',(-1.54303420125534,0.00472081811281199,
-3.47261363439072));
#6381=CARTESIAN_POINT('Ctrl Pts',(-1.54303420125534,-1.73503143864141E-18,
-3.47261363439072));
#6382=CARTESIAN_POINT('Origin',(1.4,0.,0.));
#6383=CARTESIAN_POINT('',(3.95278640450004,-0.4,-2.35922392732846E-16));
#6384=CARTESIAN_POINT('',(3.77888872553824,1.09597789965446E-16,-0.4));
#6385=CARTESIAN_POINT('Ctrl Pts',(3.95278640450004,-0.4,-2.35922392732846E-16));
#6386=CARTESIAN_POINT('Ctrl Pts',(3.95278640450004,-0.4,-0.0258360862047648));
#6387=CARTESIAN_POINT('Ctrl Pts',(3.95027516460594,-0.397512833149891,-0.0512701351527404));
#6388=CARTESIAN_POINT('Ctrl Pts',(3.9368973062695,-0.383653411095849,-0.122687402596185));
#6389=CARTESIAN_POINT('Ctrl Pts',(3.92099313571869,-0.366726070737926,-0.165860440942593));
#6390=CARTESIAN_POINT('Ctrl Pts',(3.88215383386439,-0.31747069067207,-0.248777381546757));
#6391=CARTESIAN_POINT('Ctrl Pts',(3.85821727363502,-0.282645638038343,-0.287806205063065));
#6392=CARTESIAN_POINT('Ctrl Pts',(3.81778817347559,-0.202263253170223,-0.348492766284571));
#6393=CARTESIAN_POINT('Ctrl Pts',(3.80079075477909,-0.157459904108683,-0.37127224556947));
#6394=CARTESIAN_POINT('Ctrl Pts',(3.78287958748677,-0.0731574180396009,
-0.394916332862525));
#6395=CARTESIAN_POINT('Ctrl Pts',(3.77888872553824,-0.0369000545189914,
-0.4));
#6396=CARTESIAN_POINT('Ctrl Pts',(3.77888872553824,1.94289029309402E-16,
-0.4));
#6397=CARTESIAN_POINT('',(3.77888872553824,-5.39832350745528E-17,0.4));
#6398=CARTESIAN_POINT('Ctrl Pts',(3.77888872553824,-1.17961196366423E-16,
0.4));
#6399=CARTESIAN_POINT('Ctrl Pts',(3.77888872553824,-0.0272727676506818,
0.4));
#6400=CARTESIAN_POINT('Ctrl Pts',(3.78106300168282,-0.0544020323932614,
0.397217418228499));
#6401=CARTESIAN_POINT('Ctrl Pts',(3.79271825761897,-0.127937297231108,0.381999133565693));
#6402=CARTESIAN_POINT('Ctrl Pts',(3.80621018335175,-0.171414515873833,0.36427330945719));
#6403=CARTESIAN_POINT('Ctrl Pts',(3.84417532906779,-0.259603664828111,0.309803247199999));
#6404=CARTESIAN_POINT('Ctrl Pts',(3.87017758215935,-0.300373167337263,0.269798321919243));
#6405=CARTESIAN_POINT('Ctrl Pts',(3.91068088989223,-0.354517112418169,0.189870142116222));
#6406=CARTESIAN_POINT('Ctrl Pts',(3.92708058985812,-0.372975101147337,0.151019887329265));
#6407=CARTESIAN_POINT('Ctrl Pts',(3.94744069529494,-0.394767506762619,0.0739864326554591));
#6408=CARTESIAN_POINT('Ctrl Pts',(3.95278640450004,-0.4,0.037557140405018));
#6409=CARTESIAN_POINT('Ctrl Pts',(3.95278640450004,-0.4,-2.42861286636753E-16));
#6410=CARTESIAN_POINT('',(1.54919333848297,-1.38777878078145E-17,0.4));
#6411=CARTESIAN_POINT('',(1.4,-4.89858719658941E-17,0.4));
#6412=CARTESIAN_POINT('Ctrl Pts',(1.54919333848297,-1.38777878078145E-17,
0.4));
#6413=CARTESIAN_POINT('Ctrl Pts',(1.54919333848297,0.0504597642713564,0.4));
#6414=CARTESIAN_POINT('Ctrl Pts',(1.55191545386274,0.1041286832042,0.389871621635982));
#6415=CARTESIAN_POINT('Ctrl Pts',(1.56161791111572,0.202612274012173,0.348985594046454));
#6416=CARTESIAN_POINT('Ctrl Pts',(1.56844424206536,0.247446581818911,0.318238843130327));
#6417=CARTESIAN_POINT('Ctrl Pts',(1.58115801867098,0.318233894120626,0.247451530828612));
#6418=CARTESIAN_POINT('Ctrl Pts',(1.58789001512135,0.348984503722909,0.202615161840818));
#6419=CARTESIAN_POINT('Ctrl Pts',(1.59737464039182,0.389873348412022,0.104124262326598));
#6420=CARTESIAN_POINT('Ctrl Pts',(1.6,0.4,0.0504527090972947));
#6421=CARTESIAN_POINT('Ctrl Pts',(1.6,0.4,-0.0504527090972948));
#6422=CARTESIAN_POINT('Ctrl Pts',(1.59737464039182,0.389873348412022,-0.104124262326598));
#6423=CARTESIAN_POINT('Ctrl Pts',(1.58789001512135,0.348984503722909,-0.202615161840818));
#6424=CARTESIAN_POINT('Ctrl Pts',(1.58115801867098,0.318233894120626,-0.247451530828612));
#6425=CARTESIAN_POINT('Ctrl Pts',(1.56844424206536,0.247446581818911,-0.318238843130327));
#6426=CARTESIAN_POINT('Ctrl Pts',(1.56161791111572,0.202612274012173,-0.348985594046454));
#6427=CARTESIAN_POINT('Ctrl Pts',(1.55191545386274,0.1041286832042,-0.389871621635982));
#6428=CARTESIAN_POINT('Ctrl Pts',(1.54919333848297,0.0504597642713565,-0.4));
#6429=CARTESIAN_POINT('Ctrl Pts',(1.54919333848297,-0.0504597642713564,
-0.4));
#6430=CARTESIAN_POINT('Ctrl Pts',(1.55191545386274,-0.1041286832042,-0.389871621635982));
#6431=CARTESIAN_POINT('Ctrl Pts',(1.56161791111572,-0.202612274012173,-0.348985594046454));
#6432=CARTESIAN_POINT('Ctrl Pts',(1.56844424206536,-0.247446581818911,-0.318238843130327));
#6433=CARTESIAN_POINT('Ctrl Pts',(1.58115801867098,-0.318233894120626,-0.247451530828612));
#6434=CARTESIAN_POINT('Ctrl Pts',(1.58789001512135,-0.348984503722909,-0.202615161840818));
#6435=CARTESIAN_POINT('Ctrl Pts',(1.59737464039182,-0.389873348412022,-0.104124262326598));
#6436=CARTESIAN_POINT('Ctrl Pts',(1.6,-0.4,-0.0504527090972948));
#6437=CARTESIAN_POINT('Ctrl Pts',(1.6,-0.4,0.0504527090972947));
#6438=CARTESIAN_POINT('Ctrl Pts',(1.59737464039182,-0.389873348412022,0.104124262326598));
#6439=CARTESIAN_POINT('Ctrl Pts',(1.58789001512135,-0.348984503722909,0.202615161840818));
#6440=CARTESIAN_POINT('Ctrl Pts',(1.58115801867098,-0.318233894120626,0.247451530828612));
#6441=CARTESIAN_POINT('Ctrl Pts',(1.56844424206536,-0.247446581818911,0.318238843130327));
#6442=CARTESIAN_POINT('Ctrl Pts',(1.56161791111572,-0.202612274012173,0.348985594046454));
#6443=CARTESIAN_POINT('Ctrl Pts',(1.55191545386274,-0.1041286832042,0.389871621635982));
#6444=CARTESIAN_POINT('Ctrl Pts',(1.54919333848297,-0.0504597642713564,
0.4));
#6445=CARTESIAN_POINT('Ctrl Pts',(1.54919333848297,-1.38777878078145E-17,
0.4));
#6446=CARTESIAN_POINT('Ctrl Pts',(3.77888872553824,1.86829229348027E-16,
-0.4));
#6447=CARTESIAN_POINT('Ctrl Pts',(3.77888872553824,0.00309498603048382,
-0.4));
#6448=CARTESIAN_POINT('Ctrl Pts',(3.77891661019551,0.00619449342134284,
-0.399964080504009));
#6449=CARTESIAN_POINT('Ctrl Pts',(3.77971687905484,0.0505413576531444,-0.398932950425445));
#6450=CARTESIAN_POINT('Ctrl Pts',(3.78543557857047,0.0907018003769345,-0.391648799570242));
#6451=CARTESIAN_POINT('Ctrl Pts',(3.80769137218302,0.178071320347422,-0.361944214113905));
#6452=CARTESIAN_POINT('Ctrl Pts',(3.82654127450702,0.222292530416346,-0.336211120851667));
#6453=CARTESIAN_POINT('Ctrl Pts',(3.86943599025501,0.300322258788604,-0.269500799758935));
#6454=CARTESIAN_POINT('Ctrl Pts',(3.89351725477811,0.332784356169053,-0.227832272860913));
#6455=CARTESIAN_POINT('Ctrl Pts',(3.92736856657203,0.373587746906379,-0.147954668532213));
#6456=CARTESIAN_POINT('Ctrl Pts',(3.93961646455397,0.386498097215894,-0.110669509456768));
#6457=CARTESIAN_POINT('Ctrl Pts',(3.95306292785875,0.400371072665748,-0.0337021304926297));
#6458=CARTESIAN_POINT('Ctrl Pts',(3.9545592908845,0.401808180012853,0.00409487952092722));
#6459=CARTESIAN_POINT('Ctrl Pts',(3.94603596920218,0.393166016942161,0.0855981766489427));
#6460=CARTESIAN_POINT('Ctrl Pts',(3.93468925406179,0.381660209981968,0.126674111541842));
#6461=CARTESIAN_POINT('Ctrl Pts',(3.90112046658193,0.342583173264719,0.213361732985292));
#6462=CARTESIAN_POINT('Ctrl Pts',(3.87621280158359,0.310552040291197,0.258074179286464));
#6463=CARTESIAN_POINT('Ctrl Pts',(3.83422313437239,0.237524054838919,0.324800962724505));
#6464=CARTESIAN_POINT('Ctrl Pts',(3.81668267570578,0.199892119948508,0.349479486409192));
#6465=CARTESIAN_POINT('Ctrl Pts',(3.79128132597323,0.119375494000328,0.38406200828837));
#6466=CARTESIAN_POINT('Ctrl Pts',(3.78294965429021,0.0778792943511222,0.39475779223555));
#6467=CARTESIAN_POINT('Ctrl Pts',(3.77927203108033,0.0229673800676086,0.39950680005141));
#6468=CARTESIAN_POINT('Ctrl Pts',(3.77888872553824,0.011470996564166,0.4));
#6469=CARTESIAN_POINT('Ctrl Pts',(3.77888872553824,-9.36750677027476E-17,
0.4));
#6470=CARTESIAN_POINT('Origin',(1.6,1.9,0.));
#6471=CARTESIAN_POINT('',(-1.6,1.9,-1.95943487863577E-16));
#6472=CARTESIAN_POINT('Origin',(0.,1.9,0.));
#6473=CARTESIAN_POINT('Origin',(0.,0.,0.));
#6474=CARTESIAN_POINT('',(-1.6,0.,-1.95943487863577E-16));
#6475=CARTESIAN_POINT('',(-1.6,0.,-1.95943487863577E-16));
#6476=CARTESIAN_POINT('Origin',(0.,0.,0.));
#6477=CARTESIAN_POINT('',(-4.65365783675994E-16,-7.34788079488412E-17,3.8));
#6478=CARTESIAN_POINT('Origin',(-5.38844591624835E-16,0.,4.4));
#6479=CARTESIAN_POINT('Origin',(0.,7.34788079488412E-17,0.));
#6480=CARTESIAN_POINT('Origin',(0.,7.34788079488412E-17,0.));
#6481=CARTESIAN_POINT('Origin',(0.,7.34788079488412E-17,0.));
#6482=CARTESIAN_POINT('Origin',(0.,7.34788079488412E-17,0.));
#6483=CARTESIAN_POINT('',(0.,0.,0.));
#6484=CARTESIAN_POINT('',(0.,0.,0.));
#6485=CARTESIAN_POINT('Origin',(0.4,0.18,0.38));
#6486=CARTESIAN_POINT('',(-0.8,0.2,0.36));
#6487=CARTESIAN_POINT('',(-0.8,0.16,0.4));
#6488=CARTESIAN_POINT('',(-0.8,0.2,0.36));
#6489=CARTESIAN_POINT('',(0.8,0.16,0.4));
#6490=CARTESIAN_POINT('',(0.4,0.16,0.4));
#6491=CARTESIAN_POINT('',(0.8,0.2,0.36));
#6492=CARTESIAN_POINT('',(0.8,0.16,0.4));
#6493=CARTESIAN_POINT('',(0.4,0.2,0.36));
#6494=CARTESIAN_POINT('Origin',(-0.8,0.,0.38));
#6495=CARTESIAN_POINT('',(-0.8,-0.2,0.36));
#6496=CARTESIAN_POINT('',(-0.8,-0.16,0.4));
#6497=CARTESIAN_POINT('',(-0.8,-0.2,0.36));
#6498=CARTESIAN_POINT('Origin',(-0.8,0.,0.4));
#6499=CARTESIAN_POINT('Origin',(-0.8,0.,0.36));
#6500=CARTESIAN_POINT('Origin',(-0.4,-0.18,0.38));
#6501=CARTESIAN_POINT('',(0.8,-0.2,0.36));
#6502=CARTESIAN_POINT('',(0.8,-0.16,0.4));
#6503=CARTESIAN_POINT('',(0.8,-0.2,0.36));
#6504=CARTESIAN_POINT('',(-0.4,-0.16,0.4));
#6505=CARTESIAN_POINT('',(-0.4,-0.2,0.36));
#6506=CARTESIAN_POINT('Origin',(0.8,0.,0.38));
#6507=CARTESIAN_POINT('Origin',(0.8,0.,0.4));
#6508=CARTESIAN_POINT('Origin',(0.8,0.,0.36));
#6509=CARTESIAN_POINT('Origin',(-0.8,0.,0.));
#6510=CARTESIAN_POINT('',(-0.8,0.2,0.04));
#6511=CARTESIAN_POINT('',(-0.8,0.2,0.));
#6512=CARTESIAN_POINT('',(-0.8,-0.2,0.04));
#6513=CARTESIAN_POINT('Origin',(-0.8,0.,0.04));
#6514=CARTESIAN_POINT('',(-0.8,-0.2,0.));
#6515=CARTESIAN_POINT('Origin',(0.8,0.2,0.));
#6516=CARTESIAN_POINT('',(0.8,0.2,0.04));
#6517=CARTESIAN_POINT('',(0.8,0.2,0.));
#6518=CARTESIAN_POINT('',(0.4,0.2,0.04));
#6519=CARTESIAN_POINT('Origin',(0.,0.,0.4));
#6520=CARTESIAN_POINT('Origin',(0.4,0.18,0.02));
#6521=CARTESIAN_POINT('',(-0.8,0.16,0.));
#6522=CARTESIAN_POINT('',(-0.8,0.16,0.));
#6523=CARTESIAN_POINT('',(0.8,0.16,0.));
#6524=CARTESIAN_POINT('',(0.8,0.2,0.04));
#6525=CARTESIAN_POINT('',(0.4,0.16,0.));
#6526=CARTESIAN_POINT('Origin',(-0.8,0.,0.02));
#6527=CARTESIAN_POINT('',(-0.8,-0.16,0.));
#6528=CARTESIAN_POINT('',(-0.8,-0.16,0.));
#6529=CARTESIAN_POINT('Origin',(-0.8,0.,0.));
#6530=CARTESIAN_POINT('Origin',(-0.4,-0.18,0.02));
#6531=CARTESIAN_POINT('',(0.8,-0.16,0.));
#6532=CARTESIAN_POINT('',(0.8,-0.2,0.04));
#6533=CARTESIAN_POINT('',(0.8,-0.16,0.));
#6534=CARTESIAN_POINT('',(-0.4,-0.2,0.04));
#6535=CARTESIAN_POINT('',(-0.4,-0.16,0.));
#6536=CARTESIAN_POINT('Origin',(0.8,0.,0.02));
#6537=CARTESIAN_POINT('Origin',(0.8,0.,0.04));
#6538=CARTESIAN_POINT('Origin',(0.8,0.,0.));
#6539=CARTESIAN_POINT('Origin',(0.8,0.,0.));
#6540=CARTESIAN_POINT('',(0.8,-0.2,0.));
#6541=CARTESIAN_POINT('Origin',(0.,0.,0.));
#6542=CARTESIAN_POINT('Origin',(-0.8,-0.2,0.));
#6543=CARTESIAN_POINT('',(0.,0.,0.));
#6544=CARTESIAN_POINT('Origin',(0.0866025403784439,0.,-0.15));
#6545=CARTESIAN_POINT('',(0.0866025403784439,0.,-0.15));
#6546=CARTESIAN_POINT('',(0.173205080756888,0.,0.));
#6547=CARTESIAN_POINT('',(0.142003175473055,0.,-0.0540432852445504));
#6548=CARTESIAN_POINT('',(0.0866025403784439,-0.3,-0.15));
#6549=CARTESIAN_POINT('',(0.0866025403784439,0.,-0.15));
#6550=CARTESIAN_POINT('',(0.173205080756888,-0.3,0.));
#6551=CARTESIAN_POINT('',(0.173205080756888,-0.3,0.));
#6552=CARTESIAN_POINT('',(0.173205080756888,0.,0.));
#6553=CARTESIAN_POINT('Origin',(-0.0866025403784438,0.,-0.15));
#6554=CARTESIAN_POINT('',(-0.0866025403784438,0.,-0.15));
#6555=CARTESIAN_POINT('',(0.0916987298107781,0.,-0.15));
#6556=CARTESIAN_POINT('',(-0.0866025403784438,-0.3,-0.15));
#6557=CARTESIAN_POINT('',(-0.0866025403784438,0.,-0.15));
#6558=CARTESIAN_POINT('',(0.0866025403784439,-0.3,-0.15));
#6559=CARTESIAN_POINT('Origin',(-0.173205080756888,0.,-2.77555756156289E-17));
#6560=CARTESIAN_POINT('',(-0.173205080756888,0.,-2.12115047744981E-17));
#6561=CARTESIAN_POINT('',(-0.117804445662277,0.,-0.0959567147554497));
#6562=CARTESIAN_POINT('',(-0.173205080756888,-0.3,-2.77555756156289E-17));
#6563=CARTESIAN_POINT('',(-0.173205080756888,0.,-2.12115047744981E-17));
#6564=CARTESIAN_POINT('',(-0.0866025403784438,-0.3,-0.15));
#6565=CARTESIAN_POINT('Origin',(-0.0866025403784439,0.,0.15));
#6566=CARTESIAN_POINT('',(-0.0866025403784439,0.,0.15));
#6567=CARTESIAN_POINT('',(-0.074503175473055,0.,0.17095671475545));
#6568=CARTESIAN_POINT('',(-0.0866025403784439,-0.3,0.15));
#6569=CARTESIAN_POINT('',(-0.0866025403784439,0.,0.15));
#6570=CARTESIAN_POINT('',(-0.173205080756888,-0.3,-2.12115047744981E-17));
#6571=CARTESIAN_POINT('Origin',(0.0866025403784439,0.,0.15));
#6572=CARTESIAN_POINT('',(0.0866025403784439,0.,0.15));
#6573=CARTESIAN_POINT('',(0.178301270189222,0.,0.15));
#6574=CARTESIAN_POINT('',(0.0866025403784439,-0.3,0.15));
#6575=CARTESIAN_POINT('',(0.0866025403784439,0.,0.15));
#6576=CARTESIAN_POINT('',(-0.0866025403784439,-0.3,0.15));
#6577=CARTESIAN_POINT('Origin',(0.173205080756888,0.,0.));
#6578=CARTESIAN_POINT('',(0.185304445662277,0.,-0.0209567147554496));
#6579=CARTESIAN_POINT('',(0.0866025403784439,-0.3,0.15));
#6580=CARTESIAN_POINT('Origin',(0.,-0.3,-2.77555756156289E-17));
#6581=CARTESIAN_POINT('Origin',(0.27,0.,0.));
#6582=CARTESIAN_POINT('',(-0.27,5.20417042793042E-18,-3.30654635769785E-17));
#6583=CARTESIAN_POINT('Origin',(0.,0.,0.));
#6584=CARTESIAN_POINT('Origin',(0.,-0.015,0.));
#6585=CARTESIAN_POINT('',(-0.2942,-0.0242,-3.60291088309151E-17));
#6586=CARTESIAN_POINT('Origin',(0.,-0.0242,0.));
#6587=CARTESIAN_POINT('',(-0.285,-0.015,-3.49024337756996E-17));
#6588=CARTESIAN_POINT('Origin',(0.,-0.365,0.));
#6589=CARTESIAN_POINT('',(-0.2942,-0.7058,3.60291088309151E-17));
#6590=CARTESIAN_POINT('Origin',(0.,-0.7058,0.));
#6591=CARTESIAN_POINT('',(-0.2942,-0.365,-3.60291088309151E-17));
#6592=CARTESIAN_POINT('Origin',(0.,-0.75,0.));
#6593=CARTESIAN_POINT('',(-0.2,-0.8,-2.44929359829471E-17));
#6594=CARTESIAN_POINT('Origin',(0.,-0.8,0.));
#6595=CARTESIAN_POINT('',(-0.25,-0.75,-3.06161699786838E-17));
#6596=CARTESIAN_POINT('Origin',(0.,-0.8,0.));
#6597=CARTESIAN_POINT('',(0.,0.,0.));
#6598=CARTESIAN_POINT('Origin',(0.5,0.6,0.));
#6599=CARTESIAN_POINT('',(0.561411711669787,0.6,0.2117));
#6600=CARTESIAN_POINT('Ctrl Pts',(0.561411711669787,0.6,0.2117));
#6601=CARTESIAN_POINT('Ctrl Pts',(0.561411711669787,0.573158649069562,0.2117));
#6602=CARTESIAN_POINT('Ctrl Pts',(0.563539297838208,0.544705001203387,0.206288194517509));
#6603=CARTESIAN_POINT('Ctrl Pts',(0.571006257413022,0.492626080621549,0.184616375754799));
#6604=CARTESIAN_POINT('Ctrl Pts',(0.576215579648966,0.468977868958045,0.168366880112429));
#6605=CARTESIAN_POINT('Ctrl Pts',(0.585834170098139,0.431644140867814,0.131033152022198));
#6606=CARTESIAN_POINT('Ctrl Pts',(0.590898115435695,0.41538619377614,0.107380608633747));
#6607=CARTESIAN_POINT('Ctrl Pts',(0.598025669508798,0.393708029332882,0.0552854099234836));
#6608=CARTESIAN_POINT('Ctrl Pts',(0.6,0.3883,0.0268255083819855));
#6609=CARTESIAN_POINT('Ctrl Pts',(0.6,0.3883,-0.0268255083819856));
#6610=CARTESIAN_POINT('Ctrl Pts',(0.598025669508798,0.393708029332882,-0.0552854099234837));
#6611=CARTESIAN_POINT('Ctrl Pts',(0.590898115435695,0.41538619377614,-0.107380608633747));
#6612=CARTESIAN_POINT('Ctrl Pts',(0.585834170098139,0.431644140867814,-0.131033152022198));
#6613=CARTESIAN_POINT('Ctrl Pts',(0.576215579648966,0.468977868958045,-0.168366880112429));
#6614=CARTESIAN_POINT('Ctrl Pts',(0.571006257413022,0.49262608062155,-0.184616375754799));
#6615=CARTESIAN_POINT('Ctrl Pts',(0.563539297838207,0.544705001203387,-0.206288194517509));
#6616=CARTESIAN_POINT('Ctrl Pts',(0.561411711669787,0.573158649069562,-0.2117));
#6617=CARTESIAN_POINT('Ctrl Pts',(0.561411711669787,0.626841350930438,-0.2117));
#6618=CARTESIAN_POINT('Ctrl Pts',(0.563539297838207,0.655294998796613,-0.206288194517509));
#6619=CARTESIAN_POINT('Ctrl Pts',(0.571006257413022,0.70737391937845,-0.184616375754799));
#6620=CARTESIAN_POINT('Ctrl Pts',(0.576215579648966,0.731022131041955,-0.168366880112429));
#6621=CARTESIAN_POINT('Ctrl Pts',(0.585834170098139,0.768355859132186,-0.131033152022198));
#6622=CARTESIAN_POINT('Ctrl Pts',(0.590898115435695,0.78461380622386,-0.107380608633747));
#6623=CARTESIAN_POINT('Ctrl Pts',(0.598025669508798,0.806291970667118,-0.0552854099234837));
#6624=CARTESIAN_POINT('Ctrl Pts',(0.6,0.8117,-0.0268255083819856));
#6625=CARTESIAN_POINT('Ctrl Pts',(0.6,0.8117,0.0268255083819855));
#6626=CARTESIAN_POINT('Ctrl Pts',(0.598025669508798,0.806291970667118,0.0552854099234837));
#6627=CARTESIAN_POINT('Ctrl Pts',(0.590898115435695,0.78461380622386,0.107380608633747));
#6628=CARTESIAN_POINT('Ctrl Pts',(0.585834170098139,0.768355859132186,0.131033152022198));
#6629=CARTESIAN_POINT('Ctrl Pts',(0.576215579648966,0.731022131041955,0.168366880112429));
#6630=CARTESIAN_POINT('Ctrl Pts',(0.571006257413022,0.70737391937845,0.184616375754799));
#6631=CARTESIAN_POINT('Ctrl Pts',(0.563539297838207,0.655294998796613,0.206288194517509));
#6632=CARTESIAN_POINT('Ctrl Pts',(0.561411711669787,0.626841350930438,0.2117));
#6633=CARTESIAN_POINT('Ctrl Pts',(0.561411711669787,0.6,0.2117));
#6634=CARTESIAN_POINT('',(1.07943647798284,0.6,0.2117));
#6635=CARTESIAN_POINT('',(0.5,0.6,0.2117));
#6636=CARTESIAN_POINT('Ctrl Pts',(1.07943647798284,0.6,0.2117));
#6637=CARTESIAN_POINT('Ctrl Pts',(1.07943647798284,0.626653802072043,0.2117));
#6638=CARTESIAN_POINT('Ctrl Pts',(1.08052600621577,0.655037401084091,0.206359582618511));
#6639=CARTESIAN_POINT('Ctrl Pts',(1.08443252298676,0.707175401021015,0.18473448130117));
#6640=CARTESIAN_POINT('Ctrl Pts',(1.08718996287164,0.730935702749545,0.168453308404839));
#6641=CARTESIAN_POINT('Ctrl Pts',(1.09234340045893,0.768452409692904,0.13093660146148));
#6642=CARTESIAN_POINT('Ctrl Pts',(1.09507838311905,0.784734286816328,0.107175917083711));
#6643=CARTESIAN_POINT('Ctrl Pts',(1.09893326276149,0.806359899102434,0.0550365908820453));
#6644=CARTESIAN_POINT('Ctrl Pts',(1.1,0.8117,0.0266525251200821));
#6645=CARTESIAN_POINT('Ctrl Pts',(1.1,0.8117,-0.0266525251200823));
#6646=CARTESIAN_POINT('Ctrl Pts',(1.09893326276149,0.806359899102434,-0.0550365908820454));
#6647=CARTESIAN_POINT('Ctrl Pts',(1.09507838311905,0.784734286816328,-0.107175917083711));
#6648=CARTESIAN_POINT('Ctrl Pts',(1.09234340045893,0.768452409692904,-0.130936601461481));
#6649=CARTESIAN_POINT('Ctrl Pts',(1.08718996287164,0.730935702749545,-0.16845330840484));
#6650=CARTESIAN_POINT('Ctrl Pts',(1.08443252298676,0.707175401021015,-0.18473448130117));
#6651=CARTESIAN_POINT('Ctrl Pts',(1.08052600621577,0.655037401084091,-0.206359582618511));
#6652=CARTESIAN_POINT('Ctrl Pts',(1.07943647798284,0.626653802072043,-0.2117));
#6653=CARTESIAN_POINT('Ctrl Pts',(1.07943647798284,0.573346197927957,-0.2117));
#6654=CARTESIAN_POINT('Ctrl Pts',(1.08052600621577,0.544962598915909,-0.206359582618511));
#6655=CARTESIAN_POINT('Ctrl Pts',(1.08443252298676,0.492824598978985,-0.18473448130117));
#6656=CARTESIAN_POINT('Ctrl Pts',(1.08718996287164,0.469064297250455,-0.168453308404839));
#6657=CARTESIAN_POINT('Ctrl Pts',(1.09234340045893,0.431547590307096,-0.13093660146148));
#6658=CARTESIAN_POINT('Ctrl Pts',(1.09507838311905,0.415265713183672,-0.107175917083711));
#6659=CARTESIAN_POINT('Ctrl Pts',(1.09893326276149,0.393640100897566,-0.0550365908820454));
#6660=CARTESIAN_POINT('Ctrl Pts',(1.1,0.3883,-0.0266525251200822));
#6661=CARTESIAN_POINT('Ctrl Pts',(1.1,0.3883,0.0266525251200823));
#6662=CARTESIAN_POINT('Ctrl Pts',(1.09893326276149,0.393640100897566,0.0550365908820454));
#6663=CARTESIAN_POINT('Ctrl Pts',(1.09507838311905,0.415265713183672,0.107175917083711));
#6664=CARTESIAN_POINT('Ctrl Pts',(1.09234340045893,0.431547590307096,0.13093660146148));
#6665=CARTESIAN_POINT('Ctrl Pts',(1.08718996287164,0.469064297250455,0.16845330840484));
#6666=CARTESIAN_POINT('Ctrl Pts',(1.08443252298676,0.492824598978985,0.18473448130117));
#6667=CARTESIAN_POINT('Ctrl Pts',(1.08052600621577,0.544962598915909,0.206359582618511));
#6668=CARTESIAN_POINT('Ctrl Pts',(1.07943647798284,0.573346197927957,0.2117));
#6669=CARTESIAN_POINT('Ctrl Pts',(1.07943647798284,0.6,0.2117));
#6670=CARTESIAN_POINT('Origin',(1.05,1.2,0.));
#6671=CARTESIAN_POINT('',(-1.05,1.2,-1.28587913910472E-16));
#6672=CARTESIAN_POINT('Origin',(0.,1.2,0.));
#6673=CARTESIAN_POINT('',(-0.6,1.2,-7.34788079488412E-17));
#6674=CARTESIAN_POINT('Origin',(0.,1.2,0.));
#6675=CARTESIAN_POINT('Origin',(0.,1.175,0.));
#6676=CARTESIAN_POINT('',(-1.1,1.15,-1.34711147906209E-16));
#6677=CARTESIAN_POINT('Origin',(0.,1.15,0.));
#6678=CARTESIAN_POINT('',(-1.075,1.175,-1.3164953090834E-16));
#6679=CARTESIAN_POINT('Origin',(0.,0.6,0.));
#6680=CARTESIAN_POINT('',(-1.1,0.05,-1.34711147906209E-16));
#6681=CARTESIAN_POINT('Origin',(0.,0.05,0.));
#6682=CARTESIAN_POINT('',(-1.1,0.6,-1.34711147906209E-16));
#6683=CARTESIAN_POINT('Origin',(0.,0.025,0.));
#6684=CARTESIAN_POINT('',(-1.05,-4.5102810375397E-17,-1.28587913910472E-16));
#6685=CARTESIAN_POINT('Origin',(0.,0.,0.));
#6686=CARTESIAN_POINT('',(-1.075,0.025,-1.3164953090834E-16));
#6687=CARTESIAN_POINT('Origin',(0.6,0.,0.));
#6688=CARTESIAN_POINT('',(-0.6,0.,-7.34788079488412E-17));
#6689=CARTESIAN_POINT('Origin',(0.,0.,0.));
#6690=CARTESIAN_POINT('Origin',(0.,0.6,0.));
#6691=CARTESIAN_POINT('',(-0.6,0.6,-7.34788079488412E-17));
#6692=CARTESIAN_POINT('',(0.,0.,0.));
#6693=CARTESIAN_POINT('Origin',(0.0721687836487032,0.,-0.125));
#6694=CARTESIAN_POINT('',(0.0721687836487032,0.,-0.125));
#6695=CARTESIAN_POINT('',(0.144337567297406,0.,0.));
#6696=CARTESIAN_POINT('',(0.117710979560879,0.,-0.0461186027918559));
#6697=CARTESIAN_POINT('',(0.0721687836487032,-0.25,-0.125));
#6698=CARTESIAN_POINT('',(0.0721687836487032,0.,-0.125));
#6699=CARTESIAN_POINT('',(0.144337567297406,-0.25,0.));
#6700=CARTESIAN_POINT('',(0.144337567297406,-0.25,0.));
#6701=CARTESIAN_POINT('',(0.144337567297406,0.,0.));
#6702=CARTESIAN_POINT('Origin',(-0.0721687836487032,0.,-0.125));
#6703=CARTESIAN_POINT('',(-0.0721687836487032,0.,-0.125));
#6704=CARTESIAN_POINT('',(0.0739156081756484,0.,-0.125));
#6705=CARTESIAN_POINT('',(-0.0721687836487032,-0.25,-0.125));
#6706=CARTESIAN_POINT('',(-0.0721687836487032,0.,-0.125));
#6707=CARTESIAN_POINT('',(0.0721687836487032,-0.25,-0.125));
#6708=CARTESIAN_POINT('Origin',(-0.144337567297406,0.,-4.16333634234434E-17));
#6709=CARTESIAN_POINT('',(-0.144337567297406,0.,-1.76762539787485E-17));
#6710=CARTESIAN_POINT('',(-0.0987953713852306,0.,-0.0788813972081442));
#6711=CARTESIAN_POINT('',(-0.144337567297406,-0.25,-2.77555756156289E-17));
#6712=CARTESIAN_POINT('',(-0.144337567297406,0.,-1.76762539787485E-17));
#6713=CARTESIAN_POINT('',(-0.0721687836487032,-0.25,-0.125));
#6714=CARTESIAN_POINT('Origin',(-0.0721687836487033,0.,0.125));
#6715=CARTESIAN_POINT('',(-0.0721687836487033,0.,0.125));
#6716=CARTESIAN_POINT('',(-0.0627109795608791,0.,0.141381397208144));
#6717=CARTESIAN_POINT('',(-0.0721687836487033,-0.25,0.125));
#6718=CARTESIAN_POINT('',(-0.0721687836487033,0.,0.125));
#6719=CARTESIAN_POINT('',(-0.144337567297406,-0.25,-1.76762539787485E-17));
#6720=CARTESIAN_POINT('Origin',(0.0721687836487032,0.,0.125));
#6721=CARTESIAN_POINT('',(0.0721687836487032,0.,0.125));
#6722=CARTESIAN_POINT('',(0.146084391824352,0.,0.125));
#6723=CARTESIAN_POINT('',(0.0721687836487032,-0.25,0.125));
#6724=CARTESIAN_POINT('',(0.0721687836487032,0.,0.125));
#6725=CARTESIAN_POINT('',(-0.0721687836487033,-0.25,0.125));
#6726=CARTESIAN_POINT('Origin',(0.144337567297406,0.,0.));
#6727=CARTESIAN_POINT('',(0.153795371385231,0.,-0.0163813972081441));
#6728=CARTESIAN_POINT('',(0.0721687836487032,-0.25,0.125));
#6729=CARTESIAN_POINT('Origin',(0.,-0.25,0.));
#6730=CARTESIAN_POINT('Origin',(0.22,0.,0.));
#6731=CARTESIAN_POINT('',(-0.22,-8.67361737988404E-18,-2.69422295812418E-17));
#6732=CARTESIAN_POINT('Origin',(0.,0.,0.));
#6733=CARTESIAN_POINT('Origin',(0.,-0.015,0.));
#6734=CARTESIAN_POINT('',(-0.24505,-0.02505,-3.00099698131059E-17));
#6735=CARTESIAN_POINT('Origin',(0.,-0.02505,0.));
#6736=CARTESIAN_POINT('',(-0.235,-0.015,-2.87791997799628E-17));
#6737=CARTESIAN_POINT('Origin',(0.,-0.3775,0.));
#6738=CARTESIAN_POINT('',(-0.24505,-0.72995,3.00099698131059E-17));
#6739=CARTESIAN_POINT('Origin',(0.,-0.72995,0.));
#6740=CARTESIAN_POINT('',(-0.24505,-0.3775,-3.00099698131059E-17));
#6741=CARTESIAN_POINT('Origin',(0.,-0.7625,0.));
#6742=CARTESIAN_POINT('',(-0.175,-0.8,-2.14313189850787E-17));
#6743=CARTESIAN_POINT('Origin',(0.,-0.8,0.));
#6744=CARTESIAN_POINT('',(-0.2125,-0.7625,-2.60237444818813E-17));
#6745=CARTESIAN_POINT('Origin',(0.,-0.8,0.));
#6746=CARTESIAN_POINT('',(0.,0.,0.));
#6747=CARTESIAN_POINT('',(0.,28.,7.5));
#6748=CARTESIAN_POINT('',(0.,28.,7.85));
#6749=CARTESIAN_POINT('',(-1.4,28.,7.5));
#6750=CARTESIAN_POINT('',(0.,-2.55,7.5));
#6751=CARTESIAN_POINT('',(1.4,-1.95,7.5));
#6752=CARTESIAN_POINT('',(0.,23.95,7.5));
#6753=CARTESIAN_POINT('',(1.4,24.55,7.5));
#6754=CARTESIAN_POINT('',(0.,0.,0.));
#6755=CARTESIAN_POINT('',(0.,0.,0.));
#6756=UNCERTAINTY_MEASURE_WITH_UNIT(LENGTH_MEASURE(0.001),#6806,
'DISTANCE_ACCURACY_VALUE',
'Maximum model space distance between geometric entities at asserted c
onnectivities');
#6757=UNCERTAINTY_MEASURE_WITH_UNIT(LENGTH_MEASURE(0.001),#6806,
'DISTANCE_ACCURACY_VALUE',
'Maximum model space distance between geometric entities at asserted c
onnectivities');
#6758=UNCERTAINTY_MEASURE_WITH_UNIT(LENGTH_MEASURE(0.001),#6806,
'DISTANCE_ACCURACY_VALUE',
'Maximum model space distance between geometric entities at asserted c
onnectivities');
#6759=UNCERTAINTY_MEASURE_WITH_UNIT(LENGTH_MEASURE(0.001),#6806,
'DISTANCE_ACCURACY_VALUE',
'Maximum model space distance between geometric entities at asserted c
onnectivities');
#6760=UNCERTAINTY_MEASURE_WITH_UNIT(LENGTH_MEASURE(0.001),#6806,
'DISTANCE_ACCURACY_VALUE',
'Maximum model space distance between geometric entities at asserted c
onnectivities');
#6761=UNCERTAINTY_MEASURE_WITH_UNIT(LENGTH_MEASURE(0.001),#6806,
'DISTANCE_ACCURACY_VALUE',
'Maximum model space distance between geometric entities at asserted c
onnectivities');
#6762=UNCERTAINTY_MEASURE_WITH_UNIT(LENGTH_MEASURE(0.001),#6806,
'DISTANCE_ACCURACY_VALUE',
'Maximum model space distance between geometric entities at asserted c
onnectivities');
#6763=UNCERTAINTY_MEASURE_WITH_UNIT(LENGTH_MEASURE(0.001),#6806,
'DISTANCE_ACCURACY_VALUE',
'Maximum model space distance between geometric entities at asserted c
onnectivities');
#6764=UNCERTAINTY_MEASURE_WITH_UNIT(LENGTH_MEASURE(0.001),#6806,
'DISTANCE_ACCURACY_VALUE',
'Maximum model space distance between geometric entities at asserted c
onnectivities');
#6765=UNCERTAINTY_MEASURE_WITH_UNIT(LENGTH_MEASURE(0.001),#6806,
'DISTANCE_ACCURACY_VALUE',
'Maximum model space distance between geometric entities at asserted c
onnectivities');
#6766=UNCERTAINTY_MEASURE_WITH_UNIT(LENGTH_MEASURE(0.001),#6806,
'DISTANCE_ACCURACY_VALUE',
'Maximum model space distance between geometric entities at asserted c
onnectivities');
#6767=UNCERTAINTY_MEASURE_WITH_UNIT(LENGTH_MEASURE(0.001),#6806,
'DISTANCE_ACCURACY_VALUE',
'Maximum model space distance between geometric entities at asserted c
onnectivities');
#6768=UNCERTAINTY_MEASURE_WITH_UNIT(LENGTH_MEASURE(0.001),#6806,
'DISTANCE_ACCURACY_VALUE',
'Maximum model space distance between geometric entities at asserted c
onnectivities');
#6769=UNCERTAINTY_MEASURE_WITH_UNIT(LENGTH_MEASURE(0.001),#6806,
'DISTANCE_ACCURACY_VALUE',
'Maximum model space distance between geometric entities at asserted c
onnectivities');
#6770=UNCERTAINTY_MEASURE_WITH_UNIT(LENGTH_MEASURE(0.001),#6806,
'DISTANCE_ACCURACY_VALUE',
'Maximum model space distance between geometric entities at asserted c
onnectivities');
#6771=UNCERTAINTY_MEASURE_WITH_UNIT(LENGTH_MEASURE(0.001),#6806,
'DISTANCE_ACCURACY_VALUE',
'Maximum model space distance between geometric entities at asserted c
onnectivities');
#6772=UNCERTAINTY_MEASURE_WITH_UNIT(LENGTH_MEASURE(0.001),#6806,
'DISTANCE_ACCURACY_VALUE',
'Maximum model space distance between geometric entities at asserted c
onnectivities');
#6773=UNCERTAINTY_MEASURE_WITH_UNIT(LENGTH_MEASURE(0.001),#6806,
'DISTANCE_ACCURACY_VALUE',
'Maximum model space distance between geometric entities at asserted c
onnectivities');
#6774=UNCERTAINTY_MEASURE_WITH_UNIT(LENGTH_MEASURE(0.001),#6806,
'DISTANCE_ACCURACY_VALUE',
'Maximum model space distance between geometric entities at asserted c
onnectivities');
#6775=UNCERTAINTY_MEASURE_WITH_UNIT(LENGTH_MEASURE(0.001),#6806,
'DISTANCE_ACCURACY_VALUE',
'Maximum model space distance between geometric entities at asserted c
onnectivities');
#6776=UNCERTAINTY_MEASURE_WITH_UNIT(LENGTH_MEASURE(0.001),#6806,
'DISTANCE_ACCURACY_VALUE',
'Maximum model space distance between geometric entities at asserted c
onnectivities');
#6777=UNCERTAINTY_MEASURE_WITH_UNIT(LENGTH_MEASURE(0.001),#6806,
'DISTANCE_ACCURACY_VALUE',
'Maximum model space distance between geometric entities at asserted c
onnectivities');
#6778=UNCERTAINTY_MEASURE_WITH_UNIT(LENGTH_MEASURE(0.001),#6806,
'DISTANCE_ACCURACY_VALUE',
'Maximum model space distance between geometric entities at asserted c
onnectivities');
#6779=UNCERTAINTY_MEASURE_WITH_UNIT(LENGTH_MEASURE(0.001),#6806,
'DISTANCE_ACCURACY_VALUE',
'Maximum model space distance between geometric entities at asserted c
onnectivities');
#6780=UNCERTAINTY_MEASURE_WITH_UNIT(LENGTH_MEASURE(0.001),#6806,
'DISTANCE_ACCURACY_VALUE',
'Maximum model space distance between geometric entities at asserted c
onnectivities');
#6781=(
GEOMETRIC_REPRESENTATION_CONTEXT(3)
GLOBAL_UNCERTAINTY_ASSIGNED_CONTEXT((#6756))
GLOBAL_UNIT_ASSIGNED_CONTEXT((#6806,#6808,#6809))
REPRESENTATION_CONTEXT('','3D')
);
#6782=(
GEOMETRIC_REPRESENTATION_CONTEXT(3)
GLOBAL_UNCERTAINTY_ASSIGNED_CONTEXT((#6757))
GLOBAL_UNIT_ASSIGNED_CONTEXT((#6806,#6808,#6809))
REPRESENTATION_CONTEXT('','3D')
);
#6783=(
GEOMETRIC_REPRESENTATION_CONTEXT(3)
GLOBAL_UNCERTAINTY_ASSIGNED_CONTEXT((#6758))
GLOBAL_UNIT_ASSIGNED_CONTEXT((#6806,#6808,#6809))
REPRESENTATION_CONTEXT('','3D')
);
#6784=(
GEOMETRIC_REPRESENTATION_CONTEXT(3)
GLOBAL_UNCERTAINTY_ASSIGNED_CONTEXT((#6759))
GLOBAL_UNIT_ASSIGNED_CONTEXT((#6806,#6808,#6809))
REPRESENTATION_CONTEXT('','3D')
);
#6785=(
GEOMETRIC_REPRESENTATION_CONTEXT(3)
GLOBAL_UNCERTAINTY_ASSIGNED_CONTEXT((#6760))
GLOBAL_UNIT_ASSIGNED_CONTEXT((#6806,#6808,#6809))
REPRESENTATION_CONTEXT('','3D')
);
#6786=(
GEOMETRIC_REPRESENTATION_CONTEXT(3)
GLOBAL_UNCERTAINTY_ASSIGNED_CONTEXT((#6761))
GLOBAL_UNIT_ASSIGNED_CONTEXT((#6806,#6808,#6809))
REPRESENTATION_CONTEXT('','3D')
);
#6787=(
GEOMETRIC_REPRESENTATION_CONTEXT(3)
GLOBAL_UNCERTAINTY_ASSIGNED_CONTEXT((#6762))
GLOBAL_UNIT_ASSIGNED_CONTEXT((#6806,#6808,#6809))
REPRESENTATION_CONTEXT('','3D')
);
#6788=(
GEOMETRIC_REPRESENTATION_CONTEXT(3)
GLOBAL_UNCERTAINTY_ASSIGNED_CONTEXT((#6763))
GLOBAL_UNIT_ASSIGNED_CONTEXT((#6806,#6808,#6809))
REPRESENTATION_CONTEXT('','3D')
);
#6789=(
GEOMETRIC_REPRESENTATION_CONTEXT(3)
GLOBAL_UNCERTAINTY_ASSIGNED_CONTEXT((#6764))
GLOBAL_UNIT_ASSIGNED_CONTEXT((#6806,#6808,#6809))
REPRESENTATION_CONTEXT('','3D')
);
#6790=(
GEOMETRIC_REPRESENTATION_CONTEXT(3)
GLOBAL_UNCERTAINTY_ASSIGNED_CONTEXT((#6765))
GLOBAL_UNIT_ASSIGNED_CONTEXT((#6806,#6808,#6809))
REPRESENTATION_CONTEXT('','3D')
);
#6791=(
GEOMETRIC_REPRESENTATION_CONTEXT(3)
GLOBAL_UNCERTAINTY_ASSIGNED_CONTEXT((#6766))
GLOBAL_UNIT_ASSIGNED_CONTEXT((#6806,#6808,#6809))
REPRESENTATION_CONTEXT('','3D')
);
#6792=(
GEOMETRIC_REPRESENTATION_CONTEXT(3)
GLOBAL_UNCERTAINTY_ASSIGNED_CONTEXT((#6767))
GLOBAL_UNIT_ASSIGNED_CONTEXT((#6806,#6808,#6809))
REPRESENTATION_CONTEXT('','3D')
);
#6793=(
GEOMETRIC_REPRESENTATION_CONTEXT(3)
GLOBAL_UNCERTAINTY_ASSIGNED_CONTEXT((#6768))
GLOBAL_UNIT_ASSIGNED_CONTEXT((#6806,#6808,#6809))
REPRESENTATION_CONTEXT('','3D')
);
#6794=(
GEOMETRIC_REPRESENTATION_CONTEXT(3)
GLOBAL_UNCERTAINTY_ASSIGNED_CONTEXT((#6769))
GLOBAL_UNIT_ASSIGNED_CONTEXT((#6806,#6808,#6809))
REPRESENTATION_CONTEXT('','3D')
);
#6795=(
GEOMETRIC_REPRESENTATION_CONTEXT(3)
GLOBAL_UNCERTAINTY_ASSIGNED_CONTEXT((#6770))
GLOBAL_UNIT_ASSIGNED_CONTEXT((#6806,#6808,#6809))
REPRESENTATION_CONTEXT('','3D')
);
#6796=(
GEOMETRIC_REPRESENTATION_CONTEXT(3)
GLOBAL_UNCERTAINTY_ASSIGNED_CONTEXT((#6771))
GLOBAL_UNIT_ASSIGNED_CONTEXT((#6806,#6808,#6809))
REPRESENTATION_CONTEXT('','3D')
);
#6797=(
GEOMETRIC_REPRESENTATION_CONTEXT(3)
GLOBAL_UNCERTAINTY_ASSIGNED_CONTEXT((#6772))
GLOBAL_UNIT_ASSIGNED_CONTEXT((#6806,#6808,#6809))
REPRESENTATION_CONTEXT('','3D')
);
#6798=(
GEOMETRIC_REPRESENTATION_CONTEXT(3)
GLOBAL_UNCERTAINTY_ASSIGNED_CONTEXT((#6773))
GLOBAL_UNIT_ASSIGNED_CONTEXT((#6806,#6808,#6809))
REPRESENTATION_CONTEXT('','3D')
);
#6799=(
GEOMETRIC_REPRESENTATION_CONTEXT(3)
GLOBAL_UNCERTAINTY_ASSIGNED_CONTEXT((#6774))
GLOBAL_UNIT_ASSIGNED_CONTEXT((#6806,#6808,#6809))
REPRESENTATION_CONTEXT('','3D')
);
#6800=(
GEOMETRIC_REPRESENTATION_CONTEXT(3)
GLOBAL_UNCERTAINTY_ASSIGNED_CONTEXT((#6775))
GLOBAL_UNIT_ASSIGNED_CONTEXT((#6806,#6808,#6809))
REPRESENTATION_CONTEXT('','3D')
);
#6801=(
GEOMETRIC_REPRESENTATION_CONTEXT(3)
GLOBAL_UNCERTAINTY_ASSIGNED_CONTEXT((#6776))
GLOBAL_UNIT_ASSIGNED_CONTEXT((#6806,#6808,#6809))
REPRESENTATION_CONTEXT('','3D')
);
#6802=(
GEOMETRIC_REPRESENTATION_CONTEXT(3)
GLOBAL_UNCERTAINTY_ASSIGNED_CONTEXT((#6777))
GLOBAL_UNIT_ASSIGNED_CONTEXT((#6806,#6808,#6809))
REPRESENTATION_CONTEXT('','3D')
);
#6803=(
GEOMETRIC_REPRESENTATION_CONTEXT(3)
GLOBAL_UNCERTAINTY_ASSIGNED_CONTEXT((#6778))
GLOBAL_UNIT_ASSIGNED_CONTEXT((#6806,#6808,#6809))
REPRESENTATION_CONTEXT('','3D')
);
#6804=(
GEOMETRIC_REPRESENTATION_CONTEXT(3)
GLOBAL_UNCERTAINTY_ASSIGNED_CONTEXT((#6779))
GLOBAL_UNIT_ASSIGNED_CONTEXT((#6806,#6808,#6809))
REPRESENTATION_CONTEXT('','3D')
);
#6805=(
GEOMETRIC_REPRESENTATION_CONTEXT(3)
GLOBAL_UNCERTAINTY_ASSIGNED_CONTEXT((#6780))
GLOBAL_UNIT_ASSIGNED_CONTEXT((#6806,#6808,#6809))
REPRESENTATION_CONTEXT('','3D')
);
#6806=(
LENGTH_UNIT()
NAMED_UNIT(*)
SI_UNIT(.CENTI.,.METRE.)
);
#6807=(
LENGTH_UNIT()
NAMED_UNIT(*)
SI_UNIT($,.METRE.)
);
#6808=(
NAMED_UNIT(*)
PLANE_ANGLE_UNIT()
SI_UNIT($,.RADIAN.)
);
#6809=(
NAMED_UNIT(*)
SI_UNIT($,.STERADIAN.)
SOLID_ANGLE_UNIT()
);
#6810=SHAPE_DEFINITION_REPRESENTATION(#6834,#6898);
#6811=SHAPE_DEFINITION_REPRESENTATION(#6835,#6899);
#6812=SHAPE_DEFINITION_REPRESENTATION(#6836,#6900);
#6813=SHAPE_DEFINITION_REPRESENTATION(#6837,#6901);
#6814=SHAPE_DEFINITION_REPRESENTATION(#6838,#6902);
#6815=SHAPE_DEFINITION_REPRESENTATION(#6839,#6903);
#6816=SHAPE_DEFINITION_REPRESENTATION(#6840,#6904);
#6817=SHAPE_DEFINITION_REPRESENTATION(#6841,#6905);
#6818=SHAPE_DEFINITION_REPRESENTATION(#6842,#6906);
#6819=SHAPE_DEFINITION_REPRESENTATION(#6843,#6907);
#6820=SHAPE_DEFINITION_REPRESENTATION(#6844,#6908);
#6821=SHAPE_DEFINITION_REPRESENTATION(#6845,#6909);
#6822=SHAPE_DEFINITION_REPRESENTATION(#6846,#6910);
#6823=SHAPE_DEFINITION_REPRESENTATION(#6847,#6911);
#6824=SHAPE_DEFINITION_REPRESENTATION(#6850,#6912);
#6825=SHAPE_DEFINITION_REPRESENTATION(#6851,#6913);
#6826=SHAPE_DEFINITION_REPRESENTATION(#6879,#6914);
#6827=SHAPE_DEFINITION_REPRESENTATION(#6880,#6915);
#6828=SHAPE_DEFINITION_REPRESENTATION(#6881,#6916);
#6829=SHAPE_DEFINITION_REPRESENTATION(#6882,#6917);
#6830=SHAPE_DEFINITION_REPRESENTATION(#6884,#6918);
#6831=SHAPE_DEFINITION_REPRESENTATION(#6885,#6919);
#6832=SHAPE_DEFINITION_REPRESENTATION(#6886,#6920);
#6833=SHAPE_DEFINITION_REPRESENTATION(#6887,#6921);
#6834=PRODUCT_DEFINITION_SHAPE('',$,#6923);
#6835=PRODUCT_DEFINITION_SHAPE('',$,#6924);
#6836=PRODUCT_DEFINITION_SHAPE('',$,#6925);
#6837=PRODUCT_DEFINITION_SHAPE('',$,#6926);
#6838=PRODUCT_DEFINITION_SHAPE('',$,#6927);
#6839=PRODUCT_DEFINITION_SHAPE('',$,#6928);
#6840=PRODUCT_DEFINITION_SHAPE('',$,#6929);
#6841=PRODUCT_DEFINITION_SHAPE('',$,#6930);
#6842=PRODUCT_DEFINITION_SHAPE('',$,#6931);
#6843=PRODUCT_DEFINITION_SHAPE('',$,#6932);
#6844=PRODUCT_DEFINITION_SHAPE('',$,#6933);
#6845=PRODUCT_DEFINITION_SHAPE('',$,#6934);
#6846=PRODUCT_DEFINITION_SHAPE('',$,#6935);
#6847=PRODUCT_DEFINITION_SHAPE('',$,#6936);
#6848=PRODUCT_DEFINITION_SHAPE($,$,#149);
#6849=PRODUCT_DEFINITION_SHAPE($,$,#150);
#6850=PRODUCT_DEFINITION_SHAPE('',$,#6937);
#6851=PRODUCT_DEFINITION_SHAPE('',$,#6938);
#6852=PRODUCT_DEFINITION_SHAPE($,$,#151);
#6853=PRODUCT_DEFINITION_SHAPE($,$,#152);
#6854=PRODUCT_DEFINITION_SHAPE($,$,#153);
#6855=PRODUCT_DEFINITION_SHAPE($,$,#154);
#6856=PRODUCT_DEFINITION_SHAPE($,$,#155);
#6857=PRODUCT_DEFINITION_SHAPE($,$,#156);
#6858=PRODUCT_DEFINITION_SHAPE($,$,#157);
#6859=PRODUCT_DEFINITION_SHAPE($,$,#158);
#6860=PRODUCT_DEFINITION_SHAPE($,$,#159);
#6861=PRODUCT_DEFINITION_SHAPE($,$,#160);
#6862=PRODUCT_DEFINITION_SHAPE($,$,#161);
#6863=PRODUCT_DEFINITION_SHAPE($,$,#162);
#6864=PRODUCT_DEFINITION_SHAPE($,$,#163);
#6865=PRODUCT_DEFINITION_SHAPE($,$,#164);
#6866=PRODUCT_DEFINITION_SHAPE($,$,#165);
#6867=PRODUCT_DEFINITION_SHAPE($,$,#166);
#6868=PRODUCT_DEFINITION_SHAPE($,$,#167);
#6869=PRODUCT_DEFINITION_SHAPE($,$,#168);
#6870=PRODUCT_DEFINITION_SHAPE($,$,#169);
#6871=PRODUCT_DEFINITION_SHAPE($,$,#170);
#6872=PRODUCT_DEFINITION_SHAPE($,$,#171);
#6873=PRODUCT_DEFINITION_SHAPE($,$,#172);
#6874=PRODUCT_DEFINITION_SHAPE($,$,#173);
#6875=PRODUCT_DEFINITION_SHAPE($,$,#174);
#6876=PRODUCT_DEFINITION_SHAPE($,$,#175);
#6877=PRODUCT_DEFINITION_SHAPE($,$,#176);
#6878=PRODUCT_DEFINITION_SHAPE($,$,#177);
#6879=PRODUCT_DEFINITION_SHAPE('',$,#6939);
#6880=PRODUCT_DEFINITION_SHAPE('',$,#6940);
#6881=PRODUCT_DEFINITION_SHAPE('',$,#6941);
#6882=PRODUCT_DEFINITION_SHAPE('',$,#6942);
#6883=PRODUCT_DEFINITION_SHAPE($,$,#178);
#6884=PRODUCT_DEFINITION_SHAPE('',$,#6943);
#6885=PRODUCT_DEFINITION_SHAPE('',$,#6944);
#6886=PRODUCT_DEFINITION_SHAPE('',$,#6945);
#6887=PRODUCT_DEFINITION_SHAPE('',$,#6946);
#6888=PRODUCT_DEFINITION_SHAPE($,$,#179);
#6889=PRODUCT_DEFINITION_SHAPE($,$,#180);
#6890=PRODUCT_DEFINITION_SHAPE($,$,#181);
#6891=PRODUCT_DEFINITION_SHAPE($,$,#182);
#6892=PRODUCT_DEFINITION_SHAPE($,$,#183);
#6893=PRODUCT_DEFINITION_SHAPE($,$,#184);
#6894=PRODUCT_DEFINITION_SHAPE($,$,#185);
#6895=PRODUCT_DEFINITION_SHAPE($,$,#186);
#6896=PRODUCT_DEFINITION_SHAPE($,$,#187);
#6897=PRODUCT_DEFINITION_SHAPE($,$,#188);
#6898=SHAPE_REPRESENTATION('',(#3552,#3934,#3935),#6781);
#6899=SHAPE_REPRESENTATION('',(#3553,#3778,#3779,#3780,#3781,#3782,#3783,
#3784,#3785,#3786,#3787,#3788,#3789,#3790,#3791,#3792,#3793,#3794,#3795,
#3796,#3797,#3798,#3799,#3800,#3801,#3802,#3803,#3804),#6782);
#6900=SHAPE_REPRESENTATION('',(#3554),#6783);
#6901=SHAPE_REPRESENTATION('',(#3601),#6784);
#6902=SHAPE_REPRESENTATION('',(#3610),#6785);
#6903=SHAPE_REPRESENTATION('',(#3619),#6786);
#6904=SHAPE_REPRESENTATION('',(#3628),#6787);
#6905=SHAPE_REPRESENTATION('',(#3637),#6788);
#6906=SHAPE_REPRESENTATION('',(#3646),#6789);
#6907=SHAPE_REPRESENTATION('',(#3655),#6790);
#6908=SHAPE_REPRESENTATION('',(#3664),#6791);
#6909=SHAPE_REPRESENTATION('',(#3673,#3741,#3742),#6792);
#6910=SHAPE_REPRESENTATION('',(#3674),#6793);
#6911=SHAPE_REPRESENTATION('',(#3713),#6794);
#6912=SHAPE_REPRESENTATION('',(#3743),#6795);
#6913=SHAPE_REPRESENTATION('',(#3752),#6796);
#6914=SHAPE_REPRESENTATION('',(#3805,#3926,#3927,#3928,#3929,#3930,#3931,
#3932,#3933),#6797);
#6915=SHAPE_REPRESENTATION('',(#3806),#6798);
#6916=SHAPE_REPRESENTATION('',(#3819,#3854),#6799);
#6917=SHAPE_REPRESENTATION('',(#3820),#6800);
#6918=SHAPE_REPRESENTATION('',(#3855),#6801);
#6919=SHAPE_REPRESENTATION('',(#3878),#6802);
#6920=SHAPE_REPRESENTATION('',(#3895),#6803);
#6921=SHAPE_REPRESENTATION('',(#3909),#6804);
#6922=PRODUCT_DEFINITION_CONTEXT('part definition',#6996,'design');
#6923=PRODUCT_DEFINITION('PAT-051','PAT-051',#6947,
#6922);
#6924=PRODUCT_DEFINITION('Flanged bearing frame',
'Flanged bearing frame',#6948,#6922);
#6925=PRODUCT_DEFINITION('Bearing frame','Bearing frame',#6949,#6922);
#6926=PRODUCT_DEFINITION('Flange bolt sleeve','Flange bolt sleeve',#6950,
#6922);
#6927=PRODUCT_DEFINITION('Flange bolt sleeve (1)',
'Flange bolt sleeve (1)',#6951,#6922);
#6928=PRODUCT_DEFINITION('Flange bolt sleeve (2)',
'Flange bolt sleeve (2)',#6952,#6922);
#6929=PRODUCT_DEFINITION('Flange bolt sleeve (3)',
'Flange bolt sleeve (3)',#6953,#6922);
#6930=PRODUCT_DEFINITION('Flange bolt sleeve (4)',
'Flange bolt sleeve (4)',#6954,#6922);
#6931=PRODUCT_DEFINITION('Flange bolt sleeve (5)',
'Flange bolt sleeve (5)',#6955,#6922);
#6932=PRODUCT_DEFINITION('Flange bolt sleeve (6)',
'Flange bolt sleeve (6)',#6956,#6922);
#6933=PRODUCT_DEFINITION('Flange bolt sleeve (7)',
'Flange bolt sleeve (7)',#6957,#6922);
#6934=PRODUCT_DEFINITION('Square Flange Bearing - 12 mm Bore',
'Square Flange Bearing - 12 mm Bore',#6958,#6922);
#6935=PRODUCT_DEFINITION('Housing','Housing',#6959,#6922);
#6936=PRODUCT_DEFINITION('Insert bearing','Insert bearing',#6960,#6922);
#6937=PRODUCT_DEFINITION('Flat Washer - M8','Flat Washer - M8',#6961,#6922);
#6938=PRODUCT_DEFINITION('Cap Screw - M8x30','Cap Screw - M8x30',#6962,
#6922);
#6939=PRODUCT_DEFINITION('Handwheel shaft and collars',
'Handwheel shaft and collars',#6963,#6922);
#6940=PRODUCT_DEFINITION('Handwheel shaft','Handwheel shaft',#6964,#6922);
#6941=PRODUCT_DEFINITION('Handwheel - 100 mm Diameter, 12 mm Bore',
'Handwheel - 100 mm Diameter, 12 mm Bore',#6965,#6922);
#6942=PRODUCT_DEFINITION('Revolving handle','Revolving handle',#6966,#6922);
#6943=PRODUCT_DEFINITION('Parallel Key - 4x4x20',
'Parallel Key - 4x4x20',#6967,#6922);
#6944=PRODUCT_DEFINITION('Socket Set Screw - M6x8',
'Socket Set Screw - M6x8',#6968,#6922);
#6945=PRODUCT_DEFINITION('Shaft Collar - 12 mm Bore',
'Shaft Collar - 12 mm Bore',#6969,#6922);
#6946=PRODUCT_DEFINITION('Socket Set Screw - M5x8',
'Socket Set Screw - M5x8',#6970,#6922);
#6947=PRODUCT_DEFINITION_FORMATION('',$,#6998);
#6948=PRODUCT_DEFINITION_FORMATION('',$,#6999);
#6949=PRODUCT_DEFINITION_FORMATION('',$,#7000);
#6950=PRODUCT_DEFINITION_FORMATION('',$,#7001);
#6951=PRODUCT_DEFINITION_FORMATION('',$,#7002);
#6952=PRODUCT_DEFINITION_FORMATION('',$,#7003);
#6953=PRODUCT_DEFINITION_FORMATION('',$,#7004);
#6954=PRODUCT_DEFINITION_FORMATION('',$,#7005);
#6955=PRODUCT_DEFINITION_FORMATION('',$,#7006);
#6956=PRODUCT_DEFINITION_FORMATION('',$,#7007);
#6957=PRODUCT_DEFINITION_FORMATION('',$,#7008);
#6958=PRODUCT_DEFINITION_FORMATION('',$,#7009);
#6959=PRODUCT_DEFINITION_FORMATION('',$,#7010);
#6960=PRODUCT_DEFINITION_FORMATION('',$,#7011);
#6961=PRODUCT_DEFINITION_FORMATION('',$,#7012);
#6962=PRODUCT_DEFINITION_FORMATION('',$,#7013);
#6963=PRODUCT_DEFINITION_FORMATION('',$,#7014);
#6964=PRODUCT_DEFINITION_FORMATION('',$,#7015);
#6965=PRODUCT_DEFINITION_FORMATION('',$,#7016);
#6966=PRODUCT_DEFINITION_FORMATION('',$,#7017);
#6967=PRODUCT_DEFINITION_FORMATION('',$,#7018);
#6968=PRODUCT_DEFINITION_FORMATION('',$,#7019);
#6969=PRODUCT_DEFINITION_FORMATION('',$,#7020);
#6970=PRODUCT_DEFINITION_FORMATION('',$,#7021);
#6971=PRODUCT_RELATED_PRODUCT_CATEGORY('PAT-051','PAT-051',(#6998));
#6972=PRODUCT_RELATED_PRODUCT_CATEGORY('Flanged bearing frame',
'Flanged bearing frame',(#6999));
#6973=PRODUCT_RELATED_PRODUCT_CATEGORY('Bearing frame','Bearing frame',
(#7000));
#6974=PRODUCT_RELATED_PRODUCT_CATEGORY('Flange bolt sleeve',
'Flange bolt sleeve',(#7001));
#6975=PRODUCT_RELATED_PRODUCT_CATEGORY('Flange bolt sleeve (1)',
'Flange bolt sleeve (1)',(#7002));
#6976=PRODUCT_RELATED_PRODUCT_CATEGORY('Flange bolt sleeve (2)',
'Flange bolt sleeve (2)',(#7003));
#6977=PRODUCT_RELATED_PRODUCT_CATEGORY('Flange bolt sleeve (3)',
'Flange bolt sleeve (3)',(#7004));
#6978=PRODUCT_RELATED_PRODUCT_CATEGORY('Flange bolt sleeve (4)',
'Flange bolt sleeve (4)',(#7005));
#6979=PRODUCT_RELATED_PRODUCT_CATEGORY('Flange bolt sleeve (5)',
'Flange bolt sleeve (5)',(#7006));
#6980=PRODUCT_RELATED_PRODUCT_CATEGORY('Flange bolt sleeve (6)',
'Flange bolt sleeve (6)',(#7007));
#6981=PRODUCT_RELATED_PRODUCT_CATEGORY('Flange bolt sleeve (7)',
'Flange bolt sleeve (7)',(#7008));
#6982=PRODUCT_RELATED_PRODUCT_CATEGORY(
'Square Flange Bearing - 12 mm Bore',
'Square Flange Bearing - 12 mm Bore',(#7009));
#6983=PRODUCT_RELATED_PRODUCT_CATEGORY('Housing','Housing',(#7010));
#6984=PRODUCT_RELATED_PRODUCT_CATEGORY('Insert bearing',
'Insert bearing',(#7011));
#6985=PRODUCT_RELATED_PRODUCT_CATEGORY('Flat Washer - M8',
'Flat Washer - M8',(#7012));
#6986=PRODUCT_RELATED_PRODUCT_CATEGORY('Cap Screw - M8x30',
'Cap Screw - M8x30',(#7013));
#6987=PRODUCT_RELATED_PRODUCT_CATEGORY('Handwheel shaft and collars',
'Handwheel shaft and collars',(#7014));
#6988=PRODUCT_RELATED_PRODUCT_CATEGORY('Handwheel shaft',
'Handwheel shaft',(#7015));
#6989=PRODUCT_RELATED_PRODUCT_CATEGORY(
'Handwheel - 100 mm Diameter, 12 mm Bore',
'Handwheel - 100 mm Diameter, 12 mm Bore',(#7016));
#6990=PRODUCT_RELATED_PRODUCT_CATEGORY('Revolving handle',
'Revolving handle',(#7017));
#6991=PRODUCT_RELATED_PRODUCT_CATEGORY('Parallel Key - 4x4x20',
'Parallel Key - 4x4x20',(#7018));
#6992=PRODUCT_RELATED_PRODUCT_CATEGORY('Socket Set Screw - M6x8',
'Socket Set Screw - M6x8',(#7019));
#6993=PRODUCT_RELATED_PRODUCT_CATEGORY('Shaft Collar - 12 mm Bore',
'Shaft Collar - 12 mm Bore',(#7020));
#6994=PRODUCT_RELATED_PRODUCT_CATEGORY('Socket Set Screw - M5x8',
'Socket Set Screw - M5x8',(#7021));
#6995=APPLICATION_PROTOCOL_DEFINITION('international standard',
'automotive_design',2009,#6996);
#6996=APPLICATION_CONTEXT(
'Core Data for Automotive Mechanical Design Process');
#6997=PRODUCT_CONTEXT('part definition',#6996,'mechanical');
#6998=PRODUCT('PAT-051','PAT-051',
'PAT-051',(#6997));
#6999=PRODUCT('Flanged bearing frame','Flanged bearing frame',
'Flanged bearing frame',(#6997));
#7000=PRODUCT('Bearing frame','Bearing frame','Bearing frame',(#6997));
#7001=PRODUCT('Flange bolt sleeve','Flange bolt sleeve',
'Flange bolt sleeve',(#6997));
#7002=PRODUCT('Flange bolt sleeve (1)','Flange bolt sleeve (1)',
'Flange bolt sleeve (1)',(#6997));
#7003=PRODUCT('Flange bolt sleeve (2)','Flange bolt sleeve (2)',
'Flange bolt sleeve (2)',(#6997));
#7004=PRODUCT('Flange bolt sleeve (3)','Flange bolt sleeve (3)',
'Flange bolt sleeve (3)',(#6997));
#7005=PRODUCT('Flange bolt sleeve (4)','Flange bolt sleeve (4)',
'Flange bolt sleeve (4)',(#6997));
#7006=PRODUCT('Flange bolt sleeve (5)','Flange bolt sleeve (5)',
'Flange bolt sleeve (5)',(#6997));
#7007=PRODUCT('Flange bolt sleeve (6)','Flange bolt sleeve (6)',
'Flange bolt sleeve (6)',(#6997));
#7008=PRODUCT('Flange bolt sleeve (7)','Flange bolt sleeve (7)',
'Flange bolt sleeve (7)',(#6997));
#7009=PRODUCT('Square Flange Bearing - 12 mm Bore',
'Square Flange Bearing - 12 mm Bore',
'Square Flange Bearing - 12 mm Bore',(#6997));
#7010=PRODUCT('Housing','Housing','Housing',(#6997));
#7011=PRODUCT('Insert bearing','Insert bearing','Insert bearing',(#6997));
#7012=PRODUCT('Flat Washer - M8','Flat Washer - M8','Flat Washer - M8',
(#6997));
#7013=PRODUCT('Cap Screw - M8x30','Cap Screw - M8x30',
'Cap Screw - M8x30',(#6997));
#7014=PRODUCT('Handwheel shaft and collars',
'Handwheel shaft and collars','Handwheel shaft and collars',(#6997));
#7015=PRODUCT('Handwheel shaft','Handwheel shaft','Handwheel shaft',(#6997));
#7016=PRODUCT('Handwheel - 100 mm Diameter, 12 mm Bore',
'Handwheel - 100 mm Diameter, 12 mm Bore',
'Handwheel - 100 mm Diameter, 12 mm Bore',(#6997));
#7017=PRODUCT('Revolving handle','Revolving handle','Revolving handle',
(#6997));
#7018=PRODUCT('Parallel Key - 4x4x20','Parallel Key - 4x4x20',
'Parallel Key - 4x4x20',(#6997));
#7019=PRODUCT('Socket Set Screw - M6x8','Socket Set Screw - M6x8',
'Socket Set Screw - M6x8',(#6997));
#7020=PRODUCT('Shaft Collar - 12 mm Bore','Shaft Collar - 12 mm Bore',
'Shaft Collar - 12 mm Bore',(#6997));
#7021=PRODUCT('Socket Set Screw - M5x8','Socket Set Screw - M5x8',
'Socket Set Screw - M5x8',(#6997));
#7022=PRESENTATION_STYLE_ASSIGNMENT((#7028));
#7023=PRESENTATION_STYLE_ASSIGNMENT((#7029));
#7024=PRESENTATION_STYLE_ASSIGNMENT((#7030));
#7025=PRESENTATION_STYLE_ASSIGNMENT((#7031));
#7026=PRESENTATION_STYLE_ASSIGNMENT((#7032));
#7027=PRESENTATION_STYLE_ASSIGNMENT((#7033));
#7028=SURFACE_STYLE_USAGE(.BOTH.,#7034);
#7029=SURFACE_STYLE_USAGE(.BOTH.,#7035);
#7030=SURFACE_STYLE_USAGE(.BOTH.,#7036);
#7031=SURFACE_STYLE_USAGE(.BOTH.,#7037);
#7032=SURFACE_STYLE_USAGE(.BOTH.,#7038);
#7033=SURFACE_STYLE_USAGE(.BOTH.,#7039);
#7034=SURFACE_SIDE_STYLE('',(#7040));
#7035=SURFACE_SIDE_STYLE('',(#7041));
#7036=SURFACE_SIDE_STYLE('',(#7042));
#7037=SURFACE_SIDE_STYLE('',(#7043));
#7038=SURFACE_SIDE_STYLE('',(#7044));
#7039=SURFACE_SIDE_STYLE('',(#7045));
#7040=SURFACE_STYLE_FILL_AREA(#7046);
#7041=SURFACE_STYLE_FILL_AREA(#7047);
#7042=SURFACE_STYLE_FILL_AREA(#7048);
#7043=SURFACE_STYLE_FILL_AREA(#7049);
#7044=SURFACE_STYLE_FILL_AREA(#7050);
#7045=SURFACE_STYLE_FILL_AREA(#7051);
#7046=FILL_AREA_STYLE('Steel - Satin',(#7052));
#7047=FILL_AREA_STYLE('CAD Library Painted - Steel gray',(#7053));
#7048=FILL_AREA_STYLE('CAD Library Painted - Graphite',(#7054));
#7049=FILL_AREA_STYLE('CAD Library Painted - Light blue',(#7055));
#7050=FILL_AREA_STYLE('CAD Library Painted - Engineering blue',(#7056));
#7051=FILL_AREA_STYLE('CAD Library Painted - Off white',(#7057));
#7052=FILL_AREA_STYLE_COLOUR('Steel - Satin',#7058);
#7053=FILL_AREA_STYLE_COLOUR('CAD Library Painted - Steel gray',#7059);
#7054=FILL_AREA_STYLE_COLOUR('CAD Library Painted - Graphite',#7060);
#7055=FILL_AREA_STYLE_COLOUR('CAD Library Painted - Light blue',#7061);
#7056=FILL_AREA_STYLE_COLOUR('CAD Library Painted - Engineering blue',#7062);
#7057=FILL_AREA_STYLE_COLOUR('CAD Library Painted - Off white',#7063);
#7058=COLOUR_RGB('Steel - Satin',0.627450980392157,0.627450980392157,0.627450980392157);
#7059=COLOUR_RGB('CAD Library Painted - Steel gray',0.592156862745098,0.631372549019608,
0.67843137254902);
#7060=COLOUR_RGB('CAD Library Painted - Graphite',0.0980392156862745,0.109803921568627,
0.125490196078431);
#7061=COLOUR_RGB('CAD Library Painted - Light blue',0.286274509803922,0.552941176470588,
0.780392156862745);
#7062=COLOUR_RGB('CAD Library Painted - Engineering blue',0.12156862745098,
0.356862745098039,0.6);
#7063=COLOUR_RGB('CAD Library Painted - Off white',0.909803921568627,0.901960784313726,
0.858823529411765);
#7064=COLOUR_RGB('Dark Blue',0.08,0.2,0.34);
#7065=FILL_AREA_STYLE_COLOUR('',#7064);
#7066=FILL_AREA_STYLE('',(#7065));
#7067=SURFACE_STYLE_FILL_AREA(#7066);
#7068=SURFACE_SIDE_STYLE('',(#7067));
#7069=SURFACE_STYLE_USAGE(.BOTH.,#7068);
#7070=PRESENTATION_STYLE_ASSIGNMENT((#7069));
#7071=COLOUR_RGB('Light Blue',0.38,0.62,0.78);
#7072=FILL_AREA_STYLE_COLOUR('',#7071);
#7073=FILL_AREA_STYLE('',(#7072));
#7074=SURFACE_STYLE_FILL_AREA(#7073);
#7075=SURFACE_SIDE_STYLE('',(#7074));
#7076=SURFACE_STYLE_USAGE(.BOTH.,#7075);
#7077=PRESENTATION_STYLE_ASSIGNMENT((#7076));
#7078=COLOUR_RGB('Sky Blue',0.24,0.69,0.87);
#7079=FILL_AREA_STYLE_COLOUR('',#7078);
#7080=FILL_AREA_STYLE('',(#7079));
#7081=SURFACE_STYLE_FILL_AREA(#7080);
#7082=SURFACE_SIDE_STYLE('',(#7081));
#7083=SURFACE_STYLE_USAGE(.BOTH.,#7082);
#7084=PRESENTATION_STYLE_ASSIGNMENT((#7083));
#7085=COLOUR_RGB('Grey',0.48,0.52,0.57);
#7086=FILL_AREA_STYLE_COLOUR('',#7085);
#7087=FILL_AREA_STYLE('',(#7086));
#7088=SURFACE_STYLE_FILL_AREA(#7087);
#7089=SURFACE_SIDE_STYLE('',(#7088));
#7090=SURFACE_STYLE_USAGE(.BOTH.,#7089);
#7091=PRESENTATION_STYLE_ASSIGNMENT((#7090));
#7092=COLOUR_RGB('Black',0.12,0.14,0.17);
#7093=FILL_AREA_STYLE_COLOUR('',#7092);
#7094=FILL_AREA_STYLE('',(#7093));
#7095=SURFACE_STYLE_FILL_AREA(#7094);
#7096=SURFACE_SIDE_STYLE('',(#7095));
#7097=SURFACE_STYLE_USAGE(.BOTH.,#7096);
#7098=PRESENTATION_STYLE_ASSIGNMENT((#7097));
#7099=COLOUR_RGB('Off White',0.89,0.88,0.83);
#7100=FILL_AREA_STYLE_COLOUR('',#7099);
#7101=FILL_AREA_STYLE('',(#7100));
#7102=SURFACE_STYLE_FILL_AREA(#7101);
#7103=SURFACE_SIDE_STYLE('',(#7102));
#7104=SURFACE_STYLE_USAGE(.BOTH.,#7103);
#7105=PRESENTATION_STYLE_ASSIGNMENT((#7104));
ENDSEC;
END-ISO-10303-21;
